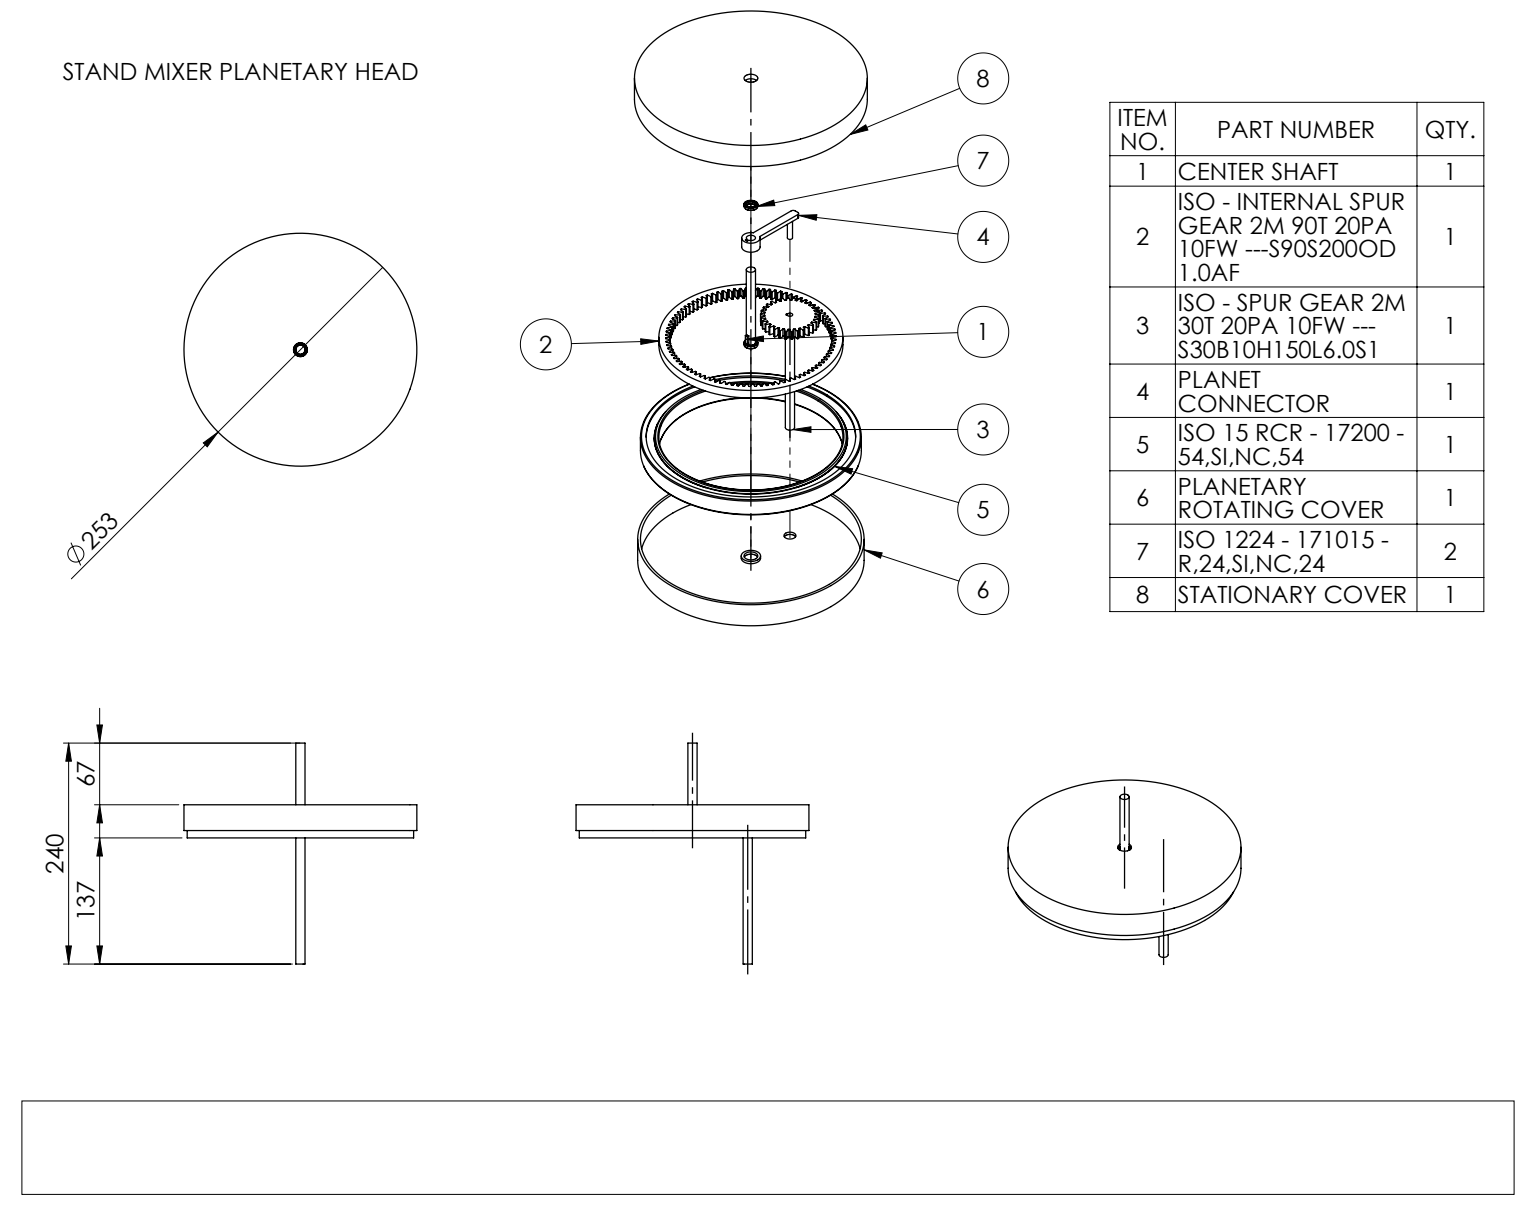
ISO-10303-21;
HEADER;
FILE_DESCRIPTION (('STEP AP214'),
    '1' );
FILE_NAME ('BR-820',
    '2026-09-30T13:58:28',
    ( '' ),
    ( '' ),
    'SwSTEP 2.0',
    'SolidWorks 2026',
    '' );
FILE_SCHEMA (( 'AUTOMOTIVE_DESIGN' ));
ENDSEC;

DATA;
#1 = VERTEX_POINT ( 'NONE', #11430 ) ;
#2 = DIRECTION ( 'NONE',  ( 1.000000000000000000, 0.000000000000000000, 0.000000000000000000 ) ) ;
#3 = ORIENTED_EDGE ( 'NONE', *, *, #13016, .T. ) ;
#4 = CARTESIAN_POINT ( 'NONE',  ( 10.00000000000000000, -41.21966518005896774, -82.80926399530329718 ) ) ;
#5 = EDGE_CURVE ( 'NONE', #21395, #6732, #6706, .T. ) ;
#6 = EDGE_CURVE ( 'NONE', #10604, #16693, #2923, .T. ) ;
#7 = EDGE_CURVE ( 'NONE', #1807, #19086, #14294, .T. ) ;
#8 = PLANE ( 'NONE',  #10324 ) ;
#9 = EDGE_CURVE ( 'NONE', #17849, #4256, #16629, .T. ) ;
#10 = DIRECTION ( 'NONE',  ( 0.000000000000000000, -0.8660254037844328234, -0.5000000000000101030 ) ) ;
#11 = DIRECTION ( 'NONE',  ( -1.000000000000000000, 0.000000000000000000, 0.000000000000000000 ) ) ;
#12 = AXIS2_PLACEMENT_3D ( 'NONE', #9946, #1451, #14823 ) ;
#13 = FACE_OUTER_BOUND ( 'NONE', #21140, .T. ) ;
#14 = CARTESIAN_POINT ( 'NONE',  ( 10.00000000000000000, 10.41137886060228901, -91.91321010181836471 ) ) ;
#15 = ORIENTED_EDGE ( 'NONE', *, *, #3774, .T. ) ;
#16 = LINE ( 'NONE', #18466, #6212 ) ;
#17 = EDGE_CURVE ( 'NONE', #14755, #17637, #4430, .T. ) ;
#18 = ORIENTED_EDGE ( 'NONE', *, *, #6903, .T. ) ;
#19 = ORIENTED_EDGE ( 'NONE', *, *, #690, .T. ) ;
#20 = ADVANCED_FACE ( 'NONE', ( #18069 ), #19725, .F. ) ;
#21 = CYLINDRICAL_SURFACE ( 'NONE', #38, 45.00000000000000000 ) ;
#22 = ORIENTED_EDGE ( 'NONE', *, *, #21258, .T. ) ;
#23 = CIRCLE ( 'NONE', #12352, 32.00000000000000000 ) ;
#24 = CYLINDRICAL_SURFACE ( 'NONE', #8070, 11.99999999999999822 ) ;
#25 = ORIENTED_EDGE ( 'NONE', *, *, #3908, .T. ) ;
#26 = ORIENTED_EDGE ( 'NONE', *, *, #547, .T. ) ;
#27 = DIRECTION ( 'NONE',  ( 0.000000000000000000, -0.2079116908177664202, 0.9781476007338040235 ) ) ;
#28 = ORIENTED_EDGE ( 'NONE', *, *, #6517, .T. ) ;
#29 = EDGE_CURVE ( 'NONE', #3387, #1233, #12896, .T. ) ;
#30 = DIRECTION ( 'NONE',  ( 1.000000000000000000, 0.000000000000000000, 0.000000000000000000 ) ) ;
#31 = EDGE_CURVE ( 'NONE', #17610, #10261, #11843, .T. ) ;
#32 = DIRECTION ( 'NONE',  ( 0.000000000000000000, 0.000000000000000000, -1.000000000000000000 ) ) ;
#33 = LINE ( 'NONE', #6780, #6309 ) ;
#34 = CARTESIAN_POINT ( 'NONE',  ( 0.000000000000000000, -19.83954325428713972, 82.71385593638686373 ) ) ;
#35 = DIRECTION ( 'NONE',  ( 0.000000000000000000, 0.000000000000000000, 1.000000000000000000 ) ) ;
#36 = CARTESIAN_POINT ( 'NONE',  ( 10.00000000000000000, 29.47587714451147534, -82.91666097089093057 ) ) ;
#37 = FACE_OUTER_BOUND ( 'NONE', #13774, .T. ) ;
#38 = AXIS2_PLACEMENT_3D ( 'NONE', #6766, #13480, #9727 ) ;
#39 = ORIENTED_EDGE ( 'NONE', *, *, #420, .F. ) ;
#40 = ADVANCED_FACE ( 'NONE', ( #13087 ), #18195, .T. ) ;
#41 = EDGE_CURVE ( 'NONE', #15664, #20418, #3042, .T. ) ;
#42 = DIRECTION ( 'NONE',  ( 0.000000000000000000, 0.000000000000000000, 1.000000000000000000 ) ) ;
#43 = DIRECTION ( 'NONE',  ( -1.000000000000000000, 0.000000000000000000, 0.000000000000000000 ) ) ;
#44 = EDGE_LOOP ( 'NONE', ( #15562, #858, #14802, #18530 ) ) ;
#45 = EDGE_CURVE ( 'NONE', #3976, #18093, #12185, .T. ) ;
#46 = DIRECTION ( 'NONE',  ( -1.000000000000000000, -0.000000000000000000, -0.000000000000000000 ) ) ;
#47 = EDGE_LOOP ( 'NONE', ( #15509, #8289, #2794, #20756 ) ) ;
#48 = EDGE_CURVE ( 'NONE', #21500, #20174, #21008, .T. ) ;
#49 = VERTEX_POINT ( 'NONE', #8229 ) ;
#50 = CARTESIAN_POINT ( 'NONE',  ( 10.00000000000000000, -19.07277123396528395, -19.80970465344768172 ) ) ;
#51 = ORIENTED_EDGE ( 'NONE', *, *, #17728, .T. ) ;
#52 = VERTEX_POINT ( 'NONE', #11320 ) ;
#53 = DIRECTION ( 'NONE',  ( -1.000000000000000000, 0.000000000000000000, -0.000000000000000000 ) ) ;
#54 = FACE_OUTER_BOUND ( 'NONE', #7670, .T. ) ;
#55 = ORIENTED_EDGE ( 'NONE', *, *, #20082, .T. ) ;
#56 = EDGE_CURVE ( 'NONE', #13601, #12425, #16433, .T. ) ;
#57 = DIRECTION ( 'NONE',  ( -1.000000000000000000, 0.000000000000000000, -0.000000000000000000 ) ) ;
#58 = DIRECTION ( 'NONE',  ( 1.000000000000000000, -0.000000000000000000, 0.000000000000000000 ) ) ;
#59 = DIRECTION ( 'NONE',  ( 1.000000000000000000, 0.000000000000000000, 0.000000000000000000 ) ) ;
#60 = DIRECTION ( 'NONE',  ( -1.000000000000000000, -0.000000000000000000, -0.000000000000000000 ) ) ;
#61 = DIRECTION ( 'NONE',  ( 0.000000000000000000, -0.5877852522924797984, 0.8090169943749425663 ) ) ;
#62 = DIRECTION ( 'NONE',  ( 1.000000000000000000, 0.000000000000000000, -0.000000000000000000 ) ) ;
#63 = ORIENTED_EDGE ( 'NONE', *, *, #8306, .T. ) ;
#64 = DIRECTION ( 'NONE',  ( 1.000000000000000000, 0.000000000000000000, 0.000000000000000000 ) ) ;
#65 = CARTESIAN_POINT ( 'NONE',  ( 10.00000000000000000, 33.95793648385814123, 86.04239391578002483 ) ) ;
#66 = CIRCLE ( 'NONE', #8534, 44.99999999999999289 ) ;
#67 = ORIENTED_EDGE ( 'NONE', *, *, #11916, .T. ) ;
#68 = DIRECTION ( 'NONE',  ( -1.000000000000000000, 0.000000000000000000, 0.000000000000000000 ) ) ;
#69 = ORIENTED_EDGE ( 'NONE', *, *, #9047, .F. ) ;
#70 = DIRECTION ( 'NONE',  ( 0.000000000000000000, 0.000000000000000000, 1.000000000000000000 ) ) ;
#71 = ORIENTED_EDGE ( 'NONE', *, *, #21788, .F. ) ;
#72 = EDGE_CURVE ( 'NONE', #17227, #7603, #6261, .T. ) ;
#73 = DIRECTION ( 'NONE',  ( 1.000000000000000000, 0.000000000000000000, 0.000000000000000000 ) ) ;
#74 = AXIS2_PLACEMENT_3D ( 'NONE', #17668, #2628, #2518 ) ;
#75 = VERTEX_POINT ( 'NONE', #9649 ) ;
#76 = ORIENTED_EDGE ( 'NONE', *, *, #8491, .T. ) ;
#77 = ORIENTED_EDGE ( 'NONE', *, *, #16610, .F. ) ;
#78 = DIRECTION ( 'NONE',  ( 1.000000000000000000, 0.000000000000000000, 0.000000000000000000 ) ) ;
#79 = ORIENTED_EDGE ( 'NONE', *, *, #6135, .T. ) ;
#80 = DIRECTION ( 'NONE',  ( 0.000000000000000000, 0.000000000000000000, 1.000000000000000000 ) ) ;
#81 = CARTESIAN_POINT ( 'NONE',  ( -1.500000000000000000, -7.000000000000000000, 15.00000000000000000 ) ) ;
#82 = DIRECTION ( 'NONE',  ( -1.000000000000000000, -0.000000000000000000, -0.000000000000000000 ) ) ;
#83 = CARTESIAN_POINT ( 'NONE',  ( 0.000000000000000000, -71.72924546249915068, -45.71766382684744201 ) ) ;
#84 = CARTESIAN_POINT ( 'NONE',  ( 10.00000000000000000, 0.000000000000000000, 0.000000000000000000 ) ) ;
#85 = AXIS2_PLACEMENT_3D ( 'NONE', #19345, #19670, #5876 ) ;
#86 = DIRECTION ( 'NONE',  ( 1.000000000000000000, 0.000000000000000000, 0.000000000000000000 ) ) ;
#87 = CARTESIAN_POINT ( 'NONE',  ( 10.00000000000000000, 0.000000000000000000, 0.000000000000000000 ) ) ;
#88 = CARTESIAN_POINT ( 'NONE',  ( 1.500000000000000000, -4.769696007084728073, 5.000000000000004441 ) ) ;
#89 = AXIS2_PLACEMENT_3D ( 'NONE', #19050, #14810, #11160 ) ;
#90 = DIRECTION ( 'NONE',  ( 1.000000000000000000, 0.000000000000000000, 0.000000000000000000 ) ) ;
#91 = CIRCLE ( 'NONE', #1856, 113.8250000000000171 ) ;
#92 = CARTESIAN_POINT ( 'NONE',  ( 0.000000000000000000, 100.0000000000000000, 0.000000000000000000 ) ) ;
#93 = ORIENTED_EDGE ( 'NONE', *, *, #13098, .F. ) ;
#94 = DIRECTION ( 'NONE',  ( -1.000000000000000000, -0.000000000000000000, -0.000000000000000000 ) ) ;
#95 = ADVANCED_FACE ( 'NONE', ( #16404 ), #1281, .F. ) ;
#96 = ORIENTED_EDGE ( 'NONE', *, *, #16353, .T. ) ;
#97 = FACE_OUTER_BOUND ( 'NONE', #19289, .T. ) ;
#98 = ORIENTED_EDGE ( 'NONE', *, *, #11209, .F. ) ;
#99 = CIRCLE ( 'NONE', #20908, 27.49900000000000233 ) ;
#100 = ORIENTED_EDGE ( 'NONE', *, *, #14180, .F. ) ;
#101 = PRODUCT_DEFINITION ( 'UNKNOWN', '', #429, #16859 ) ;
#102 = ORIENTED_EDGE ( 'NONE', *, *, #14178, .T. ) ;
#103 = CYLINDRICAL_SURFACE ( 'NONE', #17608, 88.00000000000000000 ) ;
#104 = CIRCLE ( 'NONE', #9604, 12.00000000000000000 ) ;
#105 = EDGE_LOOP ( 'NONE', ( #14807, #14622, #2671, #8655 ) ) ;
#106 = DIRECTION ( 'NONE',  ( 0.000000000000000000, 0.000000000000000000, 1.000000000000000000 ) ) ;
#107 = CARTESIAN_POINT ( 'NONE',  ( 5.000000000000000000, -30.71797041605752554, -82.46457599186584275 ) ) ;
#108 = AXIS2_PLACEMENT_3D ( 'NONE', #5672, #376, #480 ) ;
#109 = DIRECTION ( 'NONE',  ( -0.000000000000000000, -0.000000000000000000, 1.000000000000000000 ) ) ;
#110 = DIRECTION ( 'NONE',  ( -1.000000000000000000, 0.000000000000000000, 0.000000000000000000 ) ) ;
#111 = CYLINDRICAL_SURFACE ( 'NONE', #16029, 92.50100000000000477 ) ;
#112 = FACE_OUTER_BOUND ( 'NONE', #11461, .T. ) ;
#113 = DIRECTION ( 'NONE',  ( 0.000000000000000000, 0.000000000000000000, 1.000000000000000000 ) ) ;
#114 = CIRCLE ( 'NONE', #16698, 45.00000000000000711 ) ;
#115 = ORIENTED_EDGE ( 'NONE', *, *, #14200, .T. ) ;
#116 = DIRECTION ( 'NONE',  ( -1.000000000000000000, 0.000000000000000000, 0.000000000000000000 ) ) ;
#117 = CIRCLE ( 'NONE', #19528, 32.00000000000000000 ) ;
#118 = EDGE_CURVE ( 'NONE', #7770, #17965, #10413, .T. ) ;
#119 = EDGE_LOOP ( 'NONE', ( #6288, #20757, #6100, #17161 ) ) ;
#120 = CIRCLE ( 'NONE', #16359, 44.99999999999999289 ) ;
#121 = ORIENTED_EDGE ( 'NONE', *, *, #11165, .T. ) ;
#122 = CARTESIAN_POINT ( 'NONE',  ( 10.00000000000000000, 66.01871308925549897, -64.79170103522952218 ) ) ;
#123 = AXIS2_PLACEMENT_3D ( 'NONE', #20145, #6454, #4998 ) ;
#124 = ORIENTED_EDGE ( 'NONE', *, *, #16480, .F. ) ;
#125 = FACE_OUTER_BOUND ( 'NONE', #9793, .T. ) ;
#126 = ORIENTED_EDGE ( 'NONE', *, *, #4189, .T. ) ;
#127 = ORIENTED_EDGE ( 'NONE', *, *, #547, .F. ) ;
#128 = EDGE_CURVE ( 'NONE', #16693, #4447, #1608, .T. ) ;
#129 = FACE_OUTER_BOUND ( 'NONE', #11446, .T. ) ;
#130 = VECTOR ( 'NONE', #16734, 1000.000000000000000 ) ;
#131 = ORIENTED_EDGE ( 'NONE', *, *, #18244, .T. ) ;
#132 = DIRECTION ( 'NONE',  ( 0.000000000000000000, 0.000000000000000000, 1.000000000000000000 ) ) ;
#133 = EDGE_CURVE ( 'NONE', #20413, #2378, #1921, .T. ) ;
#134 = CIRCLE ( 'NONE', #12473, 5.100000000000000533 ) ;
#135 = CARTESIAN_POINT ( 'NONE',  ( -1.500000000000000000, -7.000000000000000000, 15.00000000000000000 ) ) ;
#136 = DIRECTION ( 'NONE',  ( 1.000000000000000000, 0.000000000000000000, 0.000000000000000000 ) ) ;
#137 = CARTESIAN_POINT ( 'NONE',  ( 0.000000000000000000, -36.60317927562525853, -76.78148674856802813 ) ) ;
#138 = CIRCLE ( 'NONE', #20266, 92.50100000000000477 ) ;
#139 = PLANE ( 'NONE',  #5077 ) ;
#140 = CARTESIAN_POINT ( 'NONE',  ( -90.00000000000000000, 0.000000000000000000, 0.000000000000000000 ) ) ;
#141 = DIRECTION ( 'NONE',  ( 0.000000000000000000, 0.2079116908177531808, 0.9781476007338069101 ) ) ;
#142 = VERTEX_POINT ( 'NONE', #1713 ) ;
#143 = EDGE_CURVE ( 'NONE', #8340, #1182, #890, .T. ) ;
#144 = EDGE_CURVE ( 'NONE', #2079, #18856, #6208, .T. ) ;
#145 = EDGE_CURVE ( 'NONE', #8013, #10982, #9353, .T. ) ;
#146 = DIRECTION ( 'NONE',  ( 1.000000000000000000, -0.000000000000000000, -0.000000000000000000 ) ) ;
#147 = VECTOR ( 'NONE', #20842, 1000.000000000000000 ) ;
#148 = ADVANCED_FACE ( 'NONE', ( #13522 ), #13849, .F. ) ;
#149 = CARTESIAN_POINT ( 'NONE',  ( 126.5000000000000000, 0.000000000000000000, -3.000000000000000000 ) ) ;
#150 = ORIENTED_EDGE ( 'NONE', *, *, #2176, .F. ) ;
#151 = CARTESIAN_POINT ( 'NONE',  ( 0.000000000000000000, -2.208823992044743445, 85.03123271466935762 ) ) ;
#152 = ORIENTED_EDGE ( 'NONE', *, *, #8425, .F. ) ;
#153 = CIRCLE ( 'NONE', #7560, 120.0000000000000568 ) ;
#154 = FILL_AREA_STYLE ('',( #18612 ) ) ;
#155 = VERTEX_POINT ( 'NONE', #6910 ) ;
#156 = LINE ( 'NONE', #19142, #3295 ) ;
#157 = ORIENTED_EDGE ( 'NONE', *, *, #5783, .T. ) ;
#158 = ORIENTED_EDGE ( 'NONE', *, *, #20800, .T. ) ;
#159 = CARTESIAN_POINT ( 'NONE',  ( -1.500000000000001332, 0.000000000000000000, 0.000000000000000000 ) ) ;
#160 = FACE_OUTER_BOUND ( 'NONE', #8742, .T. ) ;
#161 = ORIENTED_EDGE ( 'NONE', *, *, #12699, .T. ) ;
#162 = EDGE_CURVE ( 'NONE', #8199, #7224, #9947, .T. ) ;
#163 = VECTOR ( 'NONE', #1366, 1000.000000000000000 ) ;
#164 = CARTESIAN_POINT ( 'NONE',  ( 10.00000000000000000, 45.60224695560681596, -80.47900393021679122 ) ) ;
#165 = FACE_OUTER_BOUND ( 'NONE', #7515, .T. ) ;
#166 = AXIS2_PLACEMENT_3D ( 'NONE', #4020, #2367, #12315 ) ;
#167 = DIRECTION ( 'NONE',  ( -1.000000000000000000, -0.000000000000000000, -0.000000000000000000 ) ) ;
#168 = CARTESIAN_POINT ( 'NONE',  ( 0.000000000000000000, 0.000000000000000000, 0.000000000000000000 ) ) ;
#169 = DIRECTION ( 'NONE',  ( 1.000000000000000000, 0.000000000000000000, 0.000000000000000000 ) ) ;
#170 = EDGE_CURVE ( 'NONE', #2883, #19416, #16664, .T. ) ;
#171 = CARTESIAN_POINT ( 'NONE',  ( 5.000000000000000000, -56.05743251323904985, 67.83483072893783117 ) ) ;
#172 = AXIS2_PLACEMENT_3D ( 'NONE', #13423, #20277, #18409 ) ;
#173 = VERTEX_POINT ( 'NONE', #20274 ) ;
#174 = VECTOR ( 'NONE', #10367, 1000.000000000000000 ) ;
#175 = ADVANCED_FACE ( 'NONE', ( #54 ), #18832, .T. ) ;
#176 = CARTESIAN_POINT ( 'NONE',  ( 10.00000000000000000, 27.87320266523557777, 88.20158487341770126 ) ) ;
#177 = DIRECTION ( 'NONE',  ( -1.000000000000000000, -0.000000000000000000, -0.000000000000000000 ) ) ;
#178 = ORIENTED_EDGE ( 'NONE', *, *, #6724, .F. ) ;
#179 = DIRECTION ( 'NONE',  ( -1.000000000000000000, -0.000000000000000000, -0.000000000000000000 ) ) ;
#180 = EDGE_LOOP ( 'NONE', ( #20881, #18064, #12670, #4609 ) ) ;
#181 = AXIS2_PLACEMENT_3D ( 'NONE', #12579, #19535, #9476 ) ;
#182 = EDGE_CURVE ( 'NONE', #12268, #14735, #15959, .T. ) ;
#183 = CARTESIAN_POINT ( 'NONE',  ( 10.00000000000000000, -56.34908017029516714, -63.71789861856507997 ) ) ;
#184 = AXIS2_PLACEMENT_3D ( 'NONE', #4735, #1644, #19987 ) ;
#185 = FACE_OUTER_BOUND ( 'NONE', #19072, .T. ) ;
#186 = ORIENTED_EDGE ( 'NONE', *, *, #21572, .F. ) ;
#187 = CARTESIAN_POINT ( 'NONE',  ( 10.00000000000000000, 0.000000000000000000, 0.000000000000000000 ) ) ;
#188 = AXIS2_PLACEMENT_3D ( 'NONE', #7103, #5656, #15592 ) ;
#189 = ORIENTED_EDGE ( 'NONE', *, *, #5432, .T. ) ;
#190 = EDGE_LOOP ( 'NONE', ( #15961, #11977 ) ) ;
#191 = ORIENTED_EDGE ( 'NONE', *, *, #16743, .F. ) ;
#192 = LINE ( 'NONE', #6941, #8592 ) ;
#193 = CIRCLE ( 'NONE', #20307, 92.50100000000000477 ) ;
#194 = ORIENTED_EDGE ( 'NONE', *, *, #10939, .T. ) ;
#195 = LINE ( 'NONE', #7048, #17980 ) ;
#196 = FACE_OUTER_BOUND ( 'NONE', #2000, .T. ) ;
#197 = CARTESIAN_POINT ( 'NONE',  ( 10.00000000000000000, 75.27139873020885830, 53.76477968147838027 ) ) ;
#198 = DIRECTION ( 'NONE',  ( -1.000000000000000000, -0.000000000000000000, -0.000000000000000000 ) ) ;
#199 = CLOSED_SHELL ( 'NONE', ( #12068, #15575, #17594, #6767, #11084, #7759, #19088, #8385, #95 ) ) ;
#200 = ADVANCED_FACE ( 'NONE', ( #160 ), #12195, .F. ) ;
#201 = DIRECTION ( 'NONE',  ( -1.000000000000000000, 0.000000000000000000, 0.000000000000000000 ) ) ;
#202 = DIRECTION ( 'NONE',  ( 1.000000000000000000, 0.000000000000000000, 0.000000000000000000 ) ) ;
#203 = AXIS2_PLACEMENT_3D ( 'NONE', #2476, #711, #21255 ) ;
#204 = CARTESIAN_POINT ( 'NONE',  ( 0.000000000000000000, -65.83713140174766920, 58.39068529131174756 ) ) ;
#205 = CIRCLE ( 'NONE', #21358, 44.99999999999999289 ) ;
#206 = CARTESIAN_POINT ( 'NONE',  ( 10.00000000000000000, 0.000000000000000000, 0.000000000000000000 ) ) ;
#207 = EDGE_CURVE ( 'NONE', #13474, #6639, #1819, .T. ) ;
#208 = VECTOR ( 'NONE', #9875, 1000.000000000000000 ) ;
#209 = EDGE_CURVE ( 'NONE', #16392, #6661, #15284, .T. ) ;
#210 = FACE_OUTER_BOUND ( 'NONE', #13128, .T. ) ;
#211 = AXIS2_PLACEMENT_3D ( 'NONE', #19238, #20571, #8854 ) ;
#212 = CARTESIAN_POINT ( 'NONE',  ( 10.00000000000000888, 0.000000000000000000, 0.000000000000000000 ) ) ;
#213 = DIRECTION ( 'NONE',  ( 1.000000000000000000, 0.000000000000000000, 0.000000000000000000 ) ) ;
#214 = ORIENTED_EDGE ( 'NONE', *, *, #11490, .F. ) ;
#215 = VERTEX_POINT ( 'NONE', #17177 ) ;
#216 = LINE ( 'NONE', #10686, #17595 ) ;
#217 = ORIENTED_EDGE ( 'NONE', *, *, #17217, .F. ) ;
#218 = CIRCLE ( 'NONE', #7573, 92.50100000000000477 ) ;
#219 = EDGE_LOOP ( 'NONE', ( #5452, #14194, #8580, #6579 ) ) ;
#220 = AXIS2_PLACEMENT_3D ( 'NONE', #15734, #21034, #10973 ) ;
#221 = ORIENTED_EDGE ( 'NONE', *, *, #20358, .T. ) ;
#222 = DIRECTION ( 'NONE',  ( 0.000000000000000000, 0.000000000000000000, 1.000000000000000000 ) ) ;
#223 = ORIENTED_EDGE ( 'NONE', *, *, #9452, .F. ) ;
#224 = CARTESIAN_POINT ( 'NONE',  ( 10.00000000000000000, -81.97107881582179800, -22.71412948308650925 ) ) ;
#225 = DIRECTION ( 'NONE',  ( 0.000000000000000000, 0.000000000000000000, -1.000000000000000000 ) ) ;
#226 = CARTESIAN_POINT ( 'NONE',  ( 10.00000000000000000, 0.000000000000000000, 0.000000000000000000 ) ) ;
#227 = CARTESIAN_POINT ( 'NONE',  ( 10.00000000000000000, -27.26034713664092379, 4.817140289263571518 ) ) ;
#228 = DIRECTION ( 'NONE',  ( -1.000000000000000000, 0.000000000000000000, 0.000000000000000000 ) ) ;
#229 = CARTESIAN_POINT ( 'NONE',  ( 10.00000000000000000, 25.48117629651189375, 10.33947075754270095 ) ) ;
#230 = DIRECTION ( 'NONE',  ( 0.000000000000000000, 0.5877852522924741363, -0.8090169943749466741 ) ) ;
#231 = CIRCLE ( 'NONE', #6580, 12.00000000000000000 ) ;
#232 = ORIENTED_EDGE ( 'NONE', *, *, #45, .T. ) ;
#233 = CIRCLE ( 'NONE', #1637, 32.00000000000000000 ) ;
#234 = VECTOR ( 'NONE', #13783, 1000.000000000000000 ) ;
#235 = DIRECTION ( 'NONE',  ( -1.000000000000000000, 0.000000000000000000, 0.000000000000000000 ) ) ;
#236 = ORIENTED_EDGE ( 'NONE', *, *, #14894, .T. ) ;
#237 = ORIENTED_EDGE ( 'NONE', *, *, #7586, .T. ) ;
#238 = DIRECTION ( 'NONE',  ( 1.000000000000000000, 0.000000000000000000, 0.000000000000000000 ) ) ;
#239 = VERTEX_POINT ( 'NONE', #15611 ) ;
#240 = ORIENTED_EDGE ( 'NONE', *, *, #6283, .F. ) ;
#241 = DIRECTION ( 'NONE',  ( 0.000000000000000000, 0.000000000000000000, 1.000000000000000000 ) ) ;
#242 = ORIENTED_EDGE ( 'NONE', *, *, #31, .T. ) ;
#243 = AXIS2_PLACEMENT_3D ( 'NONE', #14900, #16894, #21541 ) ;
#244 = CIRCLE ( 'NONE', #21755, 92.50099999999999056 ) ;
#245 = DIRECTION ( 'NONE',  ( 0.000000000000000000, 0.000000000000000000, 1.000000000000000000 ) ) ;
#246 = DIRECTION ( 'NONE',  ( 0.000000000000000000, -0.4694715627858974671, 0.8829475928589232137 ) ) ;
#247 = DIRECTION ( 'NONE',  ( 1.000000000000000000, 0.000000000000000000, 0.000000000000000000 ) ) ;
#248 = EDGE_CURVE ( 'NONE', #18258, #6557, #15949, .T. ) ;
#249 = CARTESIAN_POINT ( 'NONE',  ( 10.00000000000000000, -91.49386717542229519, 13.61276130276963414 ) ) ;
#250 = CARTESIAN_POINT ( 'NONE',  ( 1.500000000000001332, 0.000000000000000000, 0.000000000000000000 ) ) ;
#251 = LINE ( 'NONE', #3457, #3152 ) ;
#252 = CYLINDRICAL_SURFACE ( 'NONE', #7349, 44.99999999999999289 ) ;
#253 = ORIENTED_EDGE ( 'NONE', *, *, #21351, .F. ) ;
#254 = EDGE_CURVE ( 'NONE', #9160, #4990, #3798, .T. ) ;
#255 = CIRCLE ( 'NONE', #10121, 11.99999999999999822 ) ;
#256 = CIRCLE ( 'NONE', #9062, 88.00000000000000000 ) ;
#257 = CIRCLE ( 'NONE', #4139, 92.50100000000001899 ) ;
#258 = DIRECTION ( 'NONE',  ( -1.000000000000000000, -0.000000000000000000, -0.000000000000000000 ) ) ;
#259 = DIRECTION ( 'NONE',  ( -1.000000000000000000, -0.000000000000000000, -0.000000000000000000 ) ) ;
#260 = ORIENTED_EDGE ( 'NONE', *, *, #20533, .T. ) ;
#261 = DIRECTION ( 'NONE',  ( -1.000000000000000000, -0.000000000000000000, -0.000000000000000000 ) ) ;
#262 = EDGE_LOOP ( 'NONE', ( #26, #4295, #8253, #16006 ) ) ;
#263 = ORIENTED_EDGE ( 'NONE', *, *, #7411, .F. ) ;
#264 = DIRECTION ( 'NONE',  ( -1.000000000000000000, -0.000000000000000000, -0.000000000000000000 ) ) ;
#265 = EDGE_LOOP ( 'NONE', ( #20128, #1055, #4125, #2694 ) ) ;
#266 = ORIENTED_EDGE ( 'NONE', *, *, #14983, .F. ) ;
#267 = CYLINDRICAL_SURFACE ( 'NONE', #10379, 44.99999999999999289 ) ;
#268 = CARTESIAN_POINT ( 'NONE',  ( 120.0000000000000000, 0.000000000000000000, -3.000000000000000000 ) ) ;
#269 = CIRCLE ( 'NONE', #5211, 44.99999999999999289 ) ;
#270 = CARTESIAN_POINT ( 'NONE',  ( 10.00000000000000000, -84.90234713953988432, 5.175025661883520200 ) ) ;
#271 = DIRECTION ( 'NONE',  ( 1.000000000000000000, 0.000000000000000000, 0.000000000000000000 ) ) ;
#272 = EDGE_CURVE ( 'NONE', #5074, #2288, #8772, .T. ) ;
#273 = CIRCLE ( 'NONE', #3803, 5.000000000000000000 ) ;
#274 = ADVANCED_FACE ( 'NONE', ( #3687 ), #15513, .F. ) ;
#275 = CARTESIAN_POINT ( 'NONE',  ( 0.000000000000000000, 0.000000000000000000, 0.000000000000000000 ) ) ;
#276 = EDGE_CURVE ( 'NONE', #11431, #4861, #15600, .T. ) ;
#277 = CARTESIAN_POINT ( 'NONE',  ( 10.00000000000000000, 0.000000000000000000, 0.000000000000000000 ) ) ;
#278 = AXIS2_PLACEMENT_3D ( 'NONE', #20316, #8268, #21854 ) ;
#279 = CARTESIAN_POINT ( 'NONE',  ( 0.000000000000000000, -61.60362715319078575, 62.84101464466223774 ) ) ;
#280 = CARTESIAN_POINT ( 'NONE',  ( 5.000000000000002665, -83.89484365856928605, 26.56417150042919673 ) ) ;
#281 = ADVANCED_FACE ( 'NONE', ( #12804 ), #21549, .F. ) ;
#282 = VERTEX_POINT ( 'NONE', #6088 ) ;
#283 = AXIS2_PLACEMENT_3D ( 'NONE', #3990, #20791, #1007 ) ;
#284 = FACE_OUTER_BOUND ( 'NONE', #6940, .T. ) ;
#285 = LINE ( 'NONE', #7031, #6929 ) ;
#286 = VERTEX_POINT ( 'NONE', #2978 ) ;
#287 = CARTESIAN_POINT ( 'NONE',  ( 5.000000000000000000, 87.96697768756401103, -2.410567674970879981 ) ) ;
#288 = EDGE_CURVE ( 'NONE', #3210, #16203, #21321, .T. ) ;
#289 = VERTEX_POINT ( 'NONE', #1331 ) ;
#290 = VECTOR ( 'NONE', #16490, 1000.000000000000000 ) ;
#291 = VECTOR ( 'NONE', #5677, 1000.000000000000000 ) ;
#292 = CARTESIAN_POINT ( 'NONE',  ( 10.00000000000000000, 0.000000000000000000, 0.000000000000000000 ) ) ;
#293 = AXIS2_PLACEMENT_3D ( 'NONE', #2385, #14534, #16196 ) ;
#294 = DIRECTION ( 'NONE',  ( -1.000000000000000000, 0.000000000000000000, 0.000000000000000000 ) ) ;
#295 = CIRCLE ( 'NONE', #15093, 7.500000000000021316 ) ;
#296 = ORIENTED_EDGE ( 'NONE', *, *, #20800, .F. ) ;
#297 = DIRECTION ( 'NONE',  ( -1.000000000000000000, -0.000000000000000000, 0.000000000000000000 ) ) ;
#298 = EDGE_CURVE ( 'NONE', #2674, #6765, #4540, .T. ) ;
#299 = ORIENTED_EDGE ( 'NONE', *, *, #7580, .F. ) ;
#300 = EDGE_LOOP ( 'NONE', ( #21001, #13570, #8396, #414 ) ) ;
#301 = VERTEX_POINT ( 'NONE', #21219 ) ;
#302 = CARTESIAN_POINT ( 'NONE',  ( -10.00000000000000888, 0.000000000000000000, 0.000000000000000000 ) ) ;
#303 = ORIENTED_EDGE ( 'NONE', *, *, #3809, .F. ) ;
#304 = CARTESIAN_POINT ( 'NONE',  ( 0.000000000000000000, 0.000000000000000000, 0.000000000000000000 ) ) ;
#305 = FACE_OUTER_BOUND ( 'NONE', #10474, .T. ) ;
#306 = DIRECTION ( 'NONE',  ( 0.000000000000000000, 0.000000000000000000, 1.000000000000000000 ) ) ;
#307 = DIRECTION ( 'NONE',  ( 1.000000000000000000, 0.000000000000000000, 0.000000000000000000 ) ) ;
#308 = DIRECTION ( 'NONE',  ( -1.000000000000000000, -0.000000000000000000, 0.000000000000000000 ) ) ;
#309 = DIRECTION ( 'NONE',  ( 1.000000000000000000, 0.000000000000000000, 0.000000000000000000 ) ) ;
#310 = CIRCLE ( 'NONE', #12639, 44.99999999999999289 ) ;
#311 = ADVANCED_FACE ( 'NONE', ( #6322 ), #16244, .F. ) ;
#312 = AXIS2_PLACEMENT_3D ( 'NONE', #17991, #11339, #16213 ) ;
#313 = CARTESIAN_POINT ( 'NONE',  ( -1.400000000000000577, 0.000000000000000000, -7.400000000000019895 ) ) ;
#314 = CARTESIAN_POINT ( 'NONE',  ( 0.000000000000000000, -46.89573839703331259, 79.73220629831473616 ) ) ;
#315 = AXIS2_PLACEMENT_3D ( 'NONE', #21324, #3204, #1444 ) ;
#316 = ORIENTED_EDGE ( 'NONE', *, *, #15812, .F. ) ;
#317 = VECTOR ( 'NONE', #1446, 1000.000000000000000 ) ;
#318 = FACE_OUTER_BOUND ( 'NONE', #13916, .T. ) ;
#319 = DIRECTION ( 'NONE',  ( 1.000000000000000000, 0.000000000000000000, 0.000000000000000000 ) ) ;
#320 = DIRECTION ( 'NONE',  ( -1.000000000000000000, -0.000000000000000000, 0.000000000000000000 ) ) ;
#321 = EDGE_CURVE ( 'NONE', #616, #3222, #16347, .T. ) ;
#322 = ORIENTED_EDGE ( 'NONE', *, *, #9631, .T. ) ;
#323 = ORIENTED_EDGE ( 'NONE', *, *, #14086, .T. ) ;
#324 = AXIS2_PLACEMENT_3D ( 'NONE', #2500, #12657, #2719 ) ;
#325 = CARTESIAN_POINT ( 'NONE',  ( 10.00000000000000000, -78.83848282823942100, 48.38314403117473006 ) ) ;
#326 = ADVANCED_FACE ( 'NONE', ( #19444 ), #4645, .F. ) ;
#327 = ORIENTED_EDGE ( 'NONE', *, *, #5685, .T. ) ;
#328 = AXIS2_PLACEMENT_3D ( 'NONE', #9035, #9242, #14226 ) ;
#329 = ORIENTED_EDGE ( 'NONE', *, *, #14866, .F. ) ;
#330 = CIRCLE ( 'NONE', #4199, 123.0000000000000000 ) ;
#331 = EDGE_CURVE ( 'NONE', #10029, #19516, #19552, .T. ) ;
#332 = AXIS2_PLACEMENT_3D ( 'NONE', #13001, #21404, #16426 ) ;
#333 = AXIS2_PLACEMENT_3D ( 'NONE', #15679, #658, #762 ) ;
#334 = ADVANCED_FACE ( 'NONE', ( #9495 ), #1106, .F. ) ;
#335 = ORIENTED_EDGE ( 'NONE', *, *, #9621, .F. ) ;
#336 = DIRECTION ( 'NONE',  ( 1.000000000000000000, 0.000000000000000000, 0.000000000000000000 ) ) ;
#337 = ORIENTED_EDGE ( 'NONE', *, *, #5445, .T. ) ;
#338 = CARTESIAN_POINT ( 'NONE',  ( 0.000000000000000000, -13.56333590713994575, -28.98337314858449076 ) ) ;
#339 = DIRECTION ( 'NONE',  ( 0.000000000000000000, -0.6946583704590034714, 0.7193398003386451967 ) ) ;
#340 = DIRECTION ( 'NONE',  ( 0.000000000000000000, 1.224646799147354933E-16, 1.000000000000000000 ) ) ;
#341 = DIRECTION ( 'NONE',  ( 1.000000000000000000, 0.000000000000000000, 0.000000000000000000 ) ) ;
#342 = EDGE_CURVE ( 'NONE', #6864, #16595, #7844, .T. ) ;
#343 = CARTESIAN_POINT ( 'NONE',  ( -5.000000000000000000, 70.00000000000000000, 9.999999999999998224 ) ) ;
#344 = CARTESIAN_POINT ( 'NONE',  ( 0.000000000000000000, 12.46320060045762013, -29.47318494484016327 ) ) ;
#345 = DIRECTION ( 'NONE',  ( 0.000000000000000000, 0.000000000000000000, -1.000000000000000000 ) ) ;
#346 = DIRECTION ( 'NONE',  ( 1.000000000000000000, -0.000000000000000000, -0.000000000000000000 ) ) ;
#347 = CIRCLE ( 'NONE', #5282, 88.00000000000000000 ) ;
#348 = AXIS2_PLACEMENT_3D ( 'NONE', #8886, #10652, #17196 ) ;
#349 = ORIENTED_EDGE ( 'NONE', *, *, #11633, .F. ) ;
#350 = DIRECTION ( 'NONE',  ( 0.000000000000000000, 0.000000000000000000, 1.000000000000000000 ) ) ;
#351 = ORIENTED_EDGE ( 'NONE', *, *, #3701, .F. ) ;
#352 = ORIENTED_EDGE ( 'NONE', *, *, #15867, .T. ) ;
#353 = DIRECTION ( 'NONE',  ( -1.000000000000000000, 0.000000000000000000, -0.000000000000000000 ) ) ;
#354 = ORIENTED_EDGE ( 'NONE', *, *, #19846, .T. ) ;
#355 = ORIENTED_EDGE ( 'NONE', *, *, #9307, .T. ) ;
#356 = CARTESIAN_POINT ( 'NONE',  ( 10.00000000000000000, 0.000000000000000000, 0.000000000000000000 ) ) ;
#357 = ORIENTED_EDGE ( 'NONE', *, *, #9039, .T. ) ;
#358 = CIRCLE ( 'NONE', #2121, 27.49900000000000944 ) ;
#359 = CIRCLE ( 'NONE', #4230, 27.49900000000000233 ) ;
#360 = DIRECTION ( 'NONE',  ( 0.000000000000000000, 0.000000000000000000, 1.000000000000000000 ) ) ;
#361 = CARTESIAN_POINT ( 'NONE',  ( 10.00000000000000000, -27.26034713664092379, -7.182859710736426706 ) ) ;
#362 = CARTESIAN_POINT ( 'NONE',  ( 10.00000000000000000, -86.77540292929711541, 14.62974526292689426 ) ) ;
#363 = DIRECTION ( 'NONE',  ( 0.000000000000000000, 0.000000000000000000, 1.000000000000000000 ) ) ;
#364 = DIRECTION ( 'NONE',  ( 0.000000000000000000, 0.000000000000000000, 1.000000000000000000 ) ) ;
#365 = DIRECTION ( 'NONE',  ( -1.000000000000000000, 0.000000000000000000, 0.000000000000000000 ) ) ;
#366 = DIRECTION ( 'NONE',  ( 0.000000000000000000, 0.5877852522924742473, -0.8090169943749465631 ) ) ;
#367 = ORIENTED_EDGE ( 'NONE', *, *, #16193, .F. ) ;
#368 = CIRCLE ( 'NONE', #4963, 44.99999999999998579 ) ;
#369 = DIRECTION ( 'NONE',  ( 0.000000000000000000, -0.8660254037844432595, 0.4999999999999920064 ) ) ;
#370 = DIRECTION ( 'NONE',  ( 1.000000000000000000, 0.000000000000000000, 0.000000000000000000 ) ) ;
#371 = ORIENTED_EDGE ( 'NONE', *, *, #13234, .F. ) ;
#372 = EDGE_CURVE ( 'NONE', #3326, #21836, #19668, .T. ) ;
#373 = DIRECTION ( 'NONE',  ( -1.000000000000000000, -0.000000000000000000, -0.000000000000000000 ) ) ;
#374 = VERTEX_POINT ( 'NONE', #17387 ) ;
#375 =( NAMED_UNIT ( * ) PLANE_ANGLE_UNIT ( ) SI_UNIT ( $, .RADIAN. ) );
#376 = DIRECTION ( 'NONE',  ( -1.000000000000000000, 0.000000000000000000, 0.000000000000000000 ) ) ;
#377 = ORIENTED_EDGE ( 'NONE', *, *, #8030, .T. ) ;
#378 = VERTEX_POINT ( 'NONE', #9266 ) ;
#379 = CARTESIAN_POINT ( 'NONE',  ( 10.00000000000000000, -57.06999622551850138, 66.98518889142063415 ) ) ;
#380 = DIRECTION ( 'NONE',  ( 1.000000000000000000, 0.000000000000000000, 0.000000000000000000 ) ) ;
#381 = PRODUCT_DEFINITION ( 'UNKNOWN', '', #13101, #3862 ) ;
#382 = CARTESIAN_POINT ( 'NONE',  ( 0.000000000000000000, -75.45728100697627383, 39.26051685139039193 ) ) ;
#383 = DIRECTION ( 'NONE',  ( 0.000000000000000000, 0.000000000000000000, 1.000000000000000000 ) ) ;
#384 = FACE_OUTER_BOUND ( 'NONE', #4779, .T. ) ;
#385 = AXIS2_PLACEMENT_3D ( 'NONE', #3175, #1301, #4716 ) ;
#386 = CYLINDRICAL_SURFACE ( 'NONE', #20961, 44.99999999999999289 ) ;
#387 = DIRECTION ( 'NONE',  ( -1.000000000000000000, -0.000000000000000000, -0.000000000000000000 ) ) ;
#388 = LINE ( 'NONE', #20601, #18757 ) ;
#389 = VERTEX_POINT ( 'NONE', #4305 ) ;
#390 = CARTESIAN_POINT ( 'NONE',  ( 0.000000000000000000, -79.66702613806754130, -29.80527447819517661 ) ) ;
#391 = ORIENTED_EDGE ( 'NONE', *, *, #16340, .T. ) ;
#392 = CARTESIAN_POINT ( 'NONE',  ( 10.00000000000000000, 19.83954325428771881, -82.71385593638672162 ) ) ;
#393 = VERTEX_POINT ( 'NONE', #883 ) ;
#394 = CARTESIAN_POINT ( 'NONE',  ( 10.00000000000000000, 28.15804365424197186, -1.358152127006073684 ) ) ;
#395 = EDGE_CURVE ( 'NONE', #9256, #19686, #11275, .T. ) ;
#396 = MECHANICAL_DESIGN_GEOMETRIC_PRESENTATION_REPRESENTATION (  '', ( #1101 ), #5694 ) ;
#397 = DIRECTION ( 'NONE',  ( 0.000000000000000000, 0.000000000000000000, -1.000000000000000000 ) ) ;
#398 = ORIENTED_EDGE ( 'NONE', *, *, #6942, .T. ) ;
#399 = ORIENTED_EDGE ( 'NONE', *, *, #18525, .T. ) ;
#400 = ORIENTED_EDGE ( 'NONE', *, *, #3209, .F. ) ;
#401 = ORIENTED_EDGE ( 'NONE', *, *, #14036, .F. ) ;
#402 = DIRECTION ( 'NONE',  ( 0.000000000000000000, -0.8660254037844328234, -0.5000000000000101030 ) ) ;
#403 = ORIENTED_EDGE ( 'NONE', *, *, #3916, .T. ) ;
#404 = DIRECTION ( 'NONE',  ( -1.000000000000000000, -0.000000000000000000, 0.000000000000000000 ) ) ;
#405 = CYLINDRICAL_SURFACE ( 'NONE', #13914, 88.00000000000000000 ) ;
#406 = DIRECTION ( 'NONE',  ( -1.000000000000000000, -0.000000000000000000, 0.000000000000000000 ) ) ;
#407 = DIRECTION ( 'NONE',  ( 1.000000000000000000, 0.000000000000000000, 0.000000000000000000 ) ) ;
#408 = DIRECTION ( 'NONE',  ( 0.000000000000000000, 0.000000000000000000, 1.000000000000000000 ) ) ;
#409 = CARTESIAN_POINT ( 'NONE',  ( 0.000000000000000000, 0.000000000000000000, 0.000000000000000000 ) ) ;
#410 = EDGE_CURVE ( 'NONE', #2166, #21782, #436, .T. ) ;
#411 = CIRCLE ( 'NONE', #3579, 113.8250000000000171 ) ;
#412 = FACE_OUTER_BOUND ( 'NONE', #20325, .T. ) ;
#413 = AXIS2_PLACEMENT_3D ( 'NONE', #19468, #6343, #19803 ) ;
#414 = ORIENTED_EDGE ( 'NONE', *, *, #12479, .F. ) ;
#415 = EDGE_CURVE ( 'NONE', #508, #14361, #20203, .T. ) ;
#416 = DIRECTION ( 'NONE',  ( -1.000000000000000000, 0.000000000000000000, -0.000000000000000000 ) ) ;
#417 = DIRECTION ( 'NONE',  ( 0.000000000000000000, 0.000000000000000000, -1.000000000000000000 ) ) ;
#418 = LINE ( 'NONE', #20634, #10815 ) ;
#419 = VERTEX_POINT ( 'NONE', #1003 ) ;
#420 = EDGE_CURVE ( 'NONE', #17054, #16203, #9590, .T. ) ;
#421 = CARTESIAN_POINT ( 'NONE',  ( -10.00000000000000000, 0.000000000000000000, 0.000000000000000000 ) ) ;
#422 = EDGE_CURVE ( 'NONE', #6705, #19466, #20900, .T. ) ;
#423 = EDGE_CURVE ( 'NONE', #1592, #10683, #10658, .T. ) ;
#424 = ORIENTED_EDGE ( 'NONE', *, *, #5191, .T. ) ;
#425 = DIRECTION ( 'NONE',  ( 1.000000000000000000, 0.000000000000000000, 0.000000000000000000 ) ) ;
#426 = EDGE_LOOP ( 'NONE', ( #2512, #10819, #21191, #16481 ) ) ;
#427 = EDGE_CURVE ( 'NONE', #19313, #4861, #15245, .T. ) ;
#428 = VERTEX_POINT ( 'NONE', #21651 ) ;
#429 = PRODUCT_DEFINITION_FORMATION_WITH_SPECIFIED_SOURCE ( 'ANY', '', #11974, .NOT_KNOWN. ) ;
#430 = ORIENTED_EDGE ( 'NONE', *, *, #8428, .T. ) ;
#431 = CARTESIAN_POINT ( 'NONE',  ( 0.000000000000000000, -40.72878876293203376, 78.00747250042435610 ) ) ;
#432 = CARTESIAN_POINT ( 'NONE',  ( 5.000000000000000000, -30.24235385705231849, -10.45944707835137777 ) ) ;
#433 = CARTESIAN_POINT ( 'NONE',  ( 10.00000000000000000, 0.000000000000000000, 0.000000000000000000 ) ) ;
#434 = CARTESIAN_POINT ( 'NONE',  ( 8.899999999999989697, 1.238117913937974620E-14, 101.1000000000000512 ) ) ;
#435 = ADVANCED_FACE ( 'NONE', ( #5083 ), #5200, .F. ) ;
#436 = CIRCLE ( 'NONE', #3254, 92.50099999999999056 ) ;
#437 = CARTESIAN_POINT ( 'NONE',  ( 10.00000000000000000, 23.10190250628953379, -89.56973317806578905 ) ) ;
#438 = DIRECTION ( 'NONE',  ( 0.000000000000000000, -0.9993908270190959842, 0.03489949670249113678 ) ) ;
#439 = CARTESIAN_POINT ( 'NONE',  ( 0.000000000000000000, 83.48638250753266732, -27.82128566055030916 ) ) ;
#440 = EDGE_CURVE ( 'NONE', #16787, #1439, #11371, .T. ) ;
#441 = CARTESIAN_POINT ( 'NONE',  ( 10.00000000000000000, 51.76708072107885528, 67.49339815138510801 ) ) ;
#442 = ADVANCED_FACE ( 'NONE', ( #4975 ), #20117, .F. ) ;
#443 = CARTESIAN_POINT ( 'NONE',  ( 0.000000000000000000, -61.71252885873428085, 58.53847642588571887 ) ) ;
#444 = ORIENTED_EDGE ( 'NONE', *, *, #1345, .F. ) ;
#445 = EDGE_CURVE ( 'NONE', #19369, #15511, #13481, .T. ) ;
#446 = DIRECTION ( 'NONE',  ( -1.000000000000000000, 0.000000000000000000, -0.000000000000000000 ) ) ;
#447 = VERTEX_POINT ( 'NONE', #4 ) ;
#448 = VECTOR ( 'NONE', #10833, 1000.000000000000000 ) ;
#449 = EDGE_LOOP ( 'NONE', ( #5641, #4304, #5239, #6868 ) ) ;
#450 = ORIENTED_EDGE ( 'NONE', *, *, #11470, .F. ) ;
#451 = DIRECTION ( 'NONE',  ( 0.000000000000000000, 0.2079116908177599532, -0.9781476007338055778 ) ) ;
#452 = EDGE_CURVE ( 'NONE', #3829, #10685, #18573, .T. ) ;
#453 = VERTEX_POINT ( 'NONE', #15229 ) ;
#454 = VERTEX_POINT ( 'NONE', #1544 ) ;
#455 = AXIS2_PLACEMENT_3D ( 'NONE', #21743, #16562, #6840 ) ;
#456 = EDGE_CURVE ( 'NONE', #2112, #5619, #7500, .T. ) ;
#457 = CARTESIAN_POINT ( 'NONE',  ( 10.00000000000000000, 0.000000000000000000, 0.000000000000000000 ) ) ;
#458 = ORIENTED_EDGE ( 'NONE', *, *, #7475, .F. ) ;
#459 = DIRECTION ( 'NONE',  ( -1.000000000000000000, -0.000000000000000000, -0.000000000000000000 ) ) ;
#460 = CARTESIAN_POINT ( 'NONE',  ( 0.000000000000000000, 83.35585896458619004, 16.94078559807978124 ) ) ;
#461 = AXIS2_PLACEMENT_3D ( 'NONE', #4977, #18458, #3312 ) ;
#462 = DIRECTION ( 'NONE',  ( 0.000000000000000000, 0.000000000000000000, 1.000000000000000000 ) ) ;
#463 = DIRECTION ( 'NONE',  ( 0.000000000000000000, 0.000000000000000000, 1.000000000000000000 ) ) ;
#464 = CARTESIAN_POINT ( 'NONE',  ( 10.00000000000000000, 81.83745710415276164, 32.35167097270178260 ) ) ;
#465 = ADVANCED_FACE ( 'NONE', ( #3425 ), #3311, .T. ) ;
#466 = DIRECTION ( 'NONE',  ( 1.000000000000000000, 0.000000000000000000, 0.000000000000000000 ) ) ;
#467 = DIRECTION ( 'NONE',  ( 1.000000000000000000, 0.000000000000000000, 0.000000000000000000 ) ) ;
#468 = CARTESIAN_POINT ( 'NONE',  ( 0.000000000000000000, 0.000000000000000000, 0.000000000000000000 ) ) ;
#469 = CIRCLE ( 'NONE', #10677, 10.49999999999999822 ) ;
#470 = CIRCLE ( 'NONE', #16293, 5.612499999999999822 ) ;
#471 = ORIENTED_EDGE ( 'NONE', *, *, #2986, .T. ) ;
#472 = CIRCLE ( 'NONE', #10698, 88.00000000000000000 ) ;
#473 = EDGE_CURVE ( 'NONE', #20811, #14806, #13136, .T. ) ;
#474 = DIRECTION ( 'NONE',  ( 1.000000000000000000, -0.000000000000000000, -0.000000000000000000 ) ) ;
#475 = CARTESIAN_POINT ( 'NONE',  ( 10.00000000000000000, 0.000000000000000000, 0.000000000000000000 ) ) ;
#476 = ORIENTED_EDGE ( 'NONE', *, *, #19100, .F. ) ;
#477 = LINE ( 'NONE', #18723, #16771 ) ;
#478 = ORIENTED_EDGE ( 'NONE', *, *, #17582, .T. ) ;
#479 = VECTOR ( 'NONE', #8463, 1000.000000000000000 ) ;
#480 = DIRECTION ( 'NONE',  ( 0.000000000000000000, 0.000000000000000000, 1.000000000000000000 ) ) ;
#481 = VERTEX_POINT ( 'NONE', #13580 ) ;
#482 = ORIENTED_EDGE ( 'NONE', *, *, #12164, .F. ) ;
#483 = CARTESIAN_POINT ( 'NONE',  ( 0.000000000000000000, 0.000000000000000000, 0.000000000000000000 ) ) ;
#484 = DIRECTION ( 'NONE',  ( -1.000000000000000000, -0.000000000000000000, 0.000000000000000000 ) ) ;
#485 = CIRCLE ( 'NONE', #20594, 104.9000000000000341 ) ;
#486 = AXIS2_PLACEMENT_3D ( 'NONE', #4785, #9859, #11408 ) ;
#487 = CARTESIAN_POINT ( 'NONE',  ( 0.000000000000000000, 0.000000000000000000, 3.000000000000000000 ) ) ;
#488 = LINE ( 'NONE', #12200, #995 ) ;
#489 = DIRECTION ( 'NONE',  ( -1.000000000000000000, 0.000000000000000000, 0.000000000000000000 ) ) ;
#490 = CARTESIAN_POINT ( 'NONE',  ( -90.00000000000000000, 0.000000000000000000, 0.000000000000000000 ) ) ;
#491 = ADVANCED_FACE ( 'NONE', ( #3094 ), #1440, .F. ) ;
#492 = CARTESIAN_POINT ( 'NONE',  ( 9.999999999999994671, 0.000000000000000000, 0.000000000000000000 ) ) ;
#493 = DIRECTION ( 'NONE',  ( 1.000000000000000000, 0.000000000000000000, -0.000000000000000000 ) ) ;
#494 = AXIS2_PLACEMENT_3D ( 'NONE', #84, #10670, #5605 ) ;
#495 = EDGE_LOOP ( 'NONE', ( #11685, #11364, #5919, #15728 ) ) ;
#496 = CARTESIAN_POINT ( 'NONE',  ( -90.00000000000000000, 0.000000000000000000, -115.1000000000000227 ) ) ;
#497 = AXIS2_PLACEMENT_3D ( 'NONE', #13069, #4792, #16173 ) ;
#498 = EDGE_LOOP ( 'NONE', ( #15179, #10420, #7326, #14605 ) ) ;
#499 = TOROIDAL_SURFACE ( 'NONE', #15302, 5.633200000000004870, 0.02570000000000143697 ) ;
#500 = DIRECTION ( 'NONE',  ( -1.000000000000000000, 0.000000000000000000, -0.000000000000000000 ) ) ;
#501 = ORIENTED_EDGE ( 'NONE', *, *, #10543, .F. ) ;
#502 = DIRECTION ( 'NONE',  ( 1.000000000000000000, 0.000000000000000000, 0.000000000000000000 ) ) ;
#503 = CARTESIAN_POINT ( 'NONE',  ( 6.123233995736766282E-16, -5.000000000000000000, 100.0000000000000000 ) ) ;
#504 = EDGE_LOOP ( 'NONE', ( #15894, #8627, #3713, #2897 ) ) ;
#505 = CIRCLE ( 'NONE', #2264, 44.99999999999998579 ) ;
#506 = ORIENTED_EDGE ( 'NONE', *, *, #19036, .F. ) ;
#507 = ORIENTED_EDGE ( 'NONE', *, *, #5060, .F. ) ;
#508 = VERTEX_POINT ( 'NONE', #9825 ) ;
#509 = CARTESIAN_POINT ( 'NONE',  ( 0.000000000000000000, 78.04699792498210797, -49.64978465107211036 ) ) ;
#510 = VERTEX_POINT ( 'NONE', #6754 ) ;
#511 = AXIS2_PLACEMENT_3D ( 'NONE', #10667, #17317, #5821 ) ;
#512 = CARTESIAN_POINT ( 'NONE',  ( -8.000000000000007105, 1.284654492305574008E-14, 104.9000000000000341 ) ) ;
#513 = DIRECTION ( 'NONE',  ( -1.000000000000000000, -0.000000000000000000, 0.000000000000000000 ) ) ;
#514 = DIRECTION ( 'NONE',  ( 0.000000000000000000, -0.9945218953682744001, 0.1045284632676437286 ) ) ;
#515 = CARTESIAN_POINT ( 'NONE',  ( 10.00000000000000000, -46.89573839703219704, -79.73220629831536144 ) ) ;
#516 = CARTESIAN_POINT ( 'NONE',  ( 0.000000000000000000, 0.000000000000000000, 0.000000000000000000 ) ) ;
#517 = EDGE_CURVE ( 'NONE', #19516, #10855, #18813, .T. ) ;
#518 = LINE ( 'NONE', #17324, #20205 ) ;
#519 = ORIENTED_EDGE ( 'NONE', *, *, #15032, .F. ) ;
#520 = CARTESIAN_POINT ( 'NONE',  ( 0.000000000000000000, -19.83954325428602061, -82.71385593638713374 ) ) ;
#521 = AXIS2_PLACEMENT_3D ( 'NONE', #551, #12365, #12467 ) ;
#522 = DIRECTION ( 'NONE',  ( 0.000000000000000000, -0.4067366430757887175, -0.9135454576426059736 ) ) ;
#523 = AXIS2_PLACEMENT_3D ( 'NONE', #5294, #8493, #10353 ) ;
#524 = EDGE_CURVE ( 'NONE', #12679, #374, #13850, .T. ) ;
#525 = CIRCLE ( 'NONE', #18926, 32.00000000000000000 ) ;
#526 = DIRECTION ( 'NONE',  ( 0.000000000000000000, -1.954455116267202870E-14, -1.000000000000000000 ) ) ;
#528 = AXIS2_PLACEMENT_3D ( 'NONE', #1902, #8639, #3779 ) ;
#527 = AXIS2_PLACEMENT_3D ( 'NONE', #18273, #14833, #16166 ) ;
#529 = ORIENTED_EDGE ( 'NONE', *, *, #2959, .T. ) ;
#530 = DIRECTION ( 'NONE',  ( 0.000000000000000000, 0.000000000000000000, -1.000000000000000000 ) ) ;
#531 = ORIENTED_EDGE ( 'NONE', *, *, #20947, .F. ) ;
#532 = DIRECTION ( 'NONE',  ( 0.000000000000000000, 0.000000000000000000, -1.000000000000000000 ) ) ;
#533 = ORIENTED_EDGE ( 'NONE', *, *, #17872, .T. ) ;
#534 = ADVANCED_FACE ( 'NONE', ( #10157 ), #3200, .F. ) ;
#535 = VERTEX_POINT ( 'NONE', #6644 ) ;
#536 = VERTEX_POINT ( 'NONE', #13466 ) ;
#537 = DIRECTION ( 'NONE',  ( 0.000000000000000000, 0.000000000000000000, 1.000000000000000000 ) ) ;
#538 = ORIENTED_EDGE ( 'NONE', *, *, #2848, .F. ) ;
#539 = DIRECTION ( 'NONE',  ( 0.000000000000000000, 0.000000000000000000, -1.000000000000000000 ) ) ;
#540 = CYLINDRICAL_SURFACE ( 'NONE', #2987, 92.50100000000000477 ) ;
#541 = CARTESIAN_POINT ( 'NONE',  ( 0.000000000000000000, 57.06999622551805373, 66.98518889142101784 ) ) ;
#542 = AXIS2_PLACEMENT_3D ( 'NONE', #21181, #2611, #6162 ) ;
#543 = AXIS2_PLACEMENT_3D ( 'NONE', #17281, #13952, #2235 ) ;
#544 = CARTESIAN_POINT ( 'NONE',  ( 0.000000000000000000, 60.00000000000000000, -15.00000000000000000 ) ) ;
#545 = AXIS2_PLACEMENT_3D ( 'NONE', #9654, #1395, #11435 ) ;
#546 = AXIS2_PLACEMENT_3D ( 'NONE', #10508, #2124, #572 ) ;
#547 = EDGE_CURVE ( 'NONE', #16474, #10634, #16910, .T. ) ;
#548 = CARTESIAN_POINT ( 'NONE',  ( 10.00000000000000000, 69.25892805976512534, 49.38005998797868301 ) ) ;
#549 = EDGE_CURVE ( 'NONE', #481, #1387, #12460, .T. ) ;
#550 = CARTESIAN_POINT ( 'NONE',  ( -5.000000000000000000, 67.00000000000000000, 15.00000000000000000 ) ) ;
#551 = CARTESIAN_POINT ( 'NONE',  ( 10.00000000000000000, 0.000000000000000000, 0.000000000000000000 ) ) ;
#552 = EDGE_CURVE ( 'NONE', #19754, #4889, #9037, .T. ) ;
#553 = DIRECTION ( 'NONE',  ( 1.000000000000000000, -0.000000000000000000, -0.000000000000000000 ) ) ;
#554 = DIRECTION ( 'NONE',  ( -1.000000000000000000, 0.000000000000000000, 0.000000000000000000 ) ) ;
#555 = EDGE_CURVE ( 'NONE', #7130, #7194, #6103, .T. ) ;
#556 = ORIENTED_EDGE ( 'NONE', *, *, #17340, .T. ) ;
#557 = FACE_OUTER_BOUND ( 'NONE', #3741, .T. ) ;
#558 = ORIENTED_EDGE ( 'NONE', *, *, #12580, .T. ) ;
#559 = ORIENTED_EDGE ( 'NONE', *, *, #2768, .F. ) ;
#560 = CIRCLE ( 'NONE', #1979, 32.00000000000000000 ) ;
#561 = ORIENTED_EDGE ( 'NONE', *, *, #20234, .T. ) ;
#562 = EDGE_CURVE ( 'NONE', #6281, #4746, #2302, .T. ) ;
#563 = AXIS2_PLACEMENT_3D ( 'NONE', #8857, #15596, #14375 ) ;
#564 = CARTESIAN_POINT ( 'NONE',  ( -10.00000000000000000, 0.000000000000000000, 0.000000000000000000 ) ) ;
#565 = ORIENTED_EDGE ( 'NONE', *, *, #7928, .T. ) ;
#566 = ORIENTED_EDGE ( 'NONE', *, *, #12735, .T. ) ;
#567 = EDGE_CURVE ( 'NONE', #14361, #6281, #9246, .T. ) ;
#568 = CARTESIAN_POINT ( 'NONE',  ( 10.00000000000000000, 86.77540292929701593, 14.62974526292747868 ) ) ;
#569 = VERTEX_POINT ( 'NONE', #15459 ) ;
#570 = CYLINDRICAL_SURFACE ( 'NONE', #13210, 92.50100000000000477 ) ;
#571 = DIRECTION ( 'NONE',  ( 0.000000000000000000, 0.000000000000000000, 1.000000000000000000 ) ) ;
#572 = DIRECTION ( 'NONE',  ( 0.000000000000000000, 0.000000000000000000, 1.000000000000000000 ) ) ;
#573 = CARTESIAN_POINT ( 'NONE',  ( -10.00000000000000000, 0.000000000000000000, 0.000000000000000000 ) ) ;
#574 = AXIS2_PLACEMENT_3D ( 'NONE', #19114, #15472, #1997 ) ;
#575 = DIRECTION ( 'NONE',  ( 0.000000000000000000, 0.000000000000000000, 1.000000000000000000 ) ) ;
#576 = AXIS2_PLACEMENT_3D ( 'NONE', #16604, #1464, #10075 ) ;
#577 = DIRECTION ( 'NONE',  ( 0.000000000000000000, 0.000000000000000000, 1.000000000000000000 ) ) ;
#578 = DIRECTION ( 'NONE',  ( 1.000000000000000000, 0.000000000000000000, 0.000000000000000000 ) ) ;
#580 = CIRCLE ( 'NONE', #5471, 44.99999999999999289 ) ;
#579 = CARTESIAN_POINT ( 'NONE',  ( 10.00000000000000000, 0.000000000000000000, 0.000000000000000000 ) ) ;
#581 = EDGE_CURVE ( 'NONE', #14715, #6477, #17390, .T. ) ;
#582 = ORIENTED_EDGE ( 'NONE', *, *, #10536, .F. ) ;
#583 = DIRECTION ( 'NONE',  ( 0.000000000000000000, 0.5299192642331999048, 0.8480480961564291764 ) ) ;
#584 = EDGE_CURVE ( 'NONE', #11040, #9927, #13903, .T. ) ;
#585 = DIRECTION ( 'NONE',  ( 0.000000000000000000, -0.5877852522924632561, -0.8090169943749546677 ) ) ;
#586 = ORIENTED_EDGE ( 'NONE', *, *, #3118, .T. ) ;
#587 = FACE_OUTER_BOUND ( 'NONE', #12213, .T. ) ;
#588 = EDGE_CURVE ( 'NONE', #8553, #4990, #15267, .T. ) ;
#589 = VERTEX_POINT ( 'NONE', #541 ) ;
#590 = VECTOR ( 'NONE', #17368, 1000.000000000000000 ) ;
#591 = CARTESIAN_POINT ( 'NONE',  ( 0.000000000000000000, 0.000000000000000000, 0.000000000000000000 ) ) ;
#592 = FACE_OUTER_BOUND ( 'NONE', #14290, .T. ) ;
#593 = ORIENTED_EDGE ( 'NONE', *, *, #19598, .F. ) ;
#594 = ORIENTED_EDGE ( 'NONE', *, *, #1930, .F. ) ;
#595 = EDGE_CURVE ( 'NONE', #18348, #18539, #20217, .T. ) ;
#596 = DIRECTION ( 'NONE',  ( -1.000000000000000000, 0.000000000000000000, -0.000000000000000000 ) ) ;
#597 = EDGE_CURVE ( 'NONE', #6613, #715, #14016, .T. ) ;
#598 = DIRECTION ( 'NONE',  ( 0.000000000000000000, -0.5877852522924632561, -0.8090169943749545567 ) ) ;
#599 = DIRECTION ( 'NONE',  ( 1.000000000000000000, 0.000000000000000000, 0.000000000000000000 ) ) ;
#600 = DIRECTION ( 'NONE',  ( 1.000000000000000000, 0.000000000000000000, 0.000000000000000000 ) ) ;
#601 = DIRECTION ( 'NONE',  ( 1.000000000000000000, 0.000000000000000000, 0.000000000000000000 ) ) ;
#602 = DIRECTION ( 'NONE',  ( -1.000000000000000000, 0.000000000000000000, 0.000000000000000000 ) ) ;
#603 = CARTESIAN_POINT ( 'NONE',  ( 0.000000000000000000, 0.000000000000000000, 0.000000000000000000 ) ) ;
#604 = VECTOR ( 'NONE', #20554, 1000.000000000000000 ) ;
#605 = VECTOR ( 'NONE', #3170, 1000.000000000000000 ) ;
#606 = ORIENTED_EDGE ( 'NONE', *, *, #10944, .F. ) ;
#607 = DIRECTION ( 'NONE',  ( 0.000000000000000000, 0.000000000000000000, 1.000000000000000000 ) ) ;
#608 = ORIENTED_EDGE ( 'NONE', *, *, #11246, .T. ) ;
#609 = CARTESIAN_POINT ( 'NONE',  ( 10.00000000000000000, 14.02138820415029663, -83.89630571862271324 ) ) ;
#610 = VERTEX_POINT ( 'NONE', #10481 ) ;
#611 = DIRECTION ( 'NONE',  ( 0.000000000000000000, 0.000000000000000000, 1.000000000000000000 ) ) ;
#612 = FACE_OUTER_BOUND ( 'NONE', #18647, .T. ) ;
#613 = ORIENTED_EDGE ( 'NONE', *, *, #13922, .F. ) ;
#614 = CIRCLE ( 'NONE', #16845, 44.99999999999999289 ) ;
#615 = EDGE_LOOP ( 'NONE', ( #5922, #19113 ) ) ;
#616 = VERTEX_POINT ( 'NONE', #12037 ) ;
#617 = AXIS2_PLACEMENT_3D ( 'NONE', #12857, #4142, #19606 ) ;
#618 = ORIENTED_EDGE ( 'NONE', *, *, #20802, .T. ) ;
#619 = CARTESIAN_POINT ( 'NONE',  ( 0.000000000000000000, -27.07404830566974141, 4.815694066514342175 ) ) ;
#620 = LINE ( 'NONE', #11105, #13677 ) ;
#621 = CIRCLE ( 'NONE', #16136, 92.50100000000001899 ) ;
#622 = ORIENTED_EDGE ( 'NONE', *, *, #14710, .F. ) ;
#623 = DIRECTION ( 'NONE',  ( 1.000000000000000000, -0.000000000000000000, -0.000000000000000000 ) ) ;
#624 = DIRECTION ( 'NONE',  ( -0.000000000000000000, 0.000000000000000000, 1.000000000000000000 ) ) ;
#625 = CARTESIAN_POINT ( 'NONE',  ( 0.000000000000000000, 41.21966518005955038, 82.80926399530301296 ) ) ;
#626 = CARTESIAN_POINT ( 'NONE',  ( 7.440711023145602176, 0.000000000000000000, 0.000000000000000000 ) ) ;
#627 = DIRECTION ( 'NONE',  ( -1.000000000000000000, -0.000000000000000000, 0.000000000000000000 ) ) ;
#628 = VERTEX_POINT ( 'NONE', #13806 ) ;
#629 = CARTESIAN_POINT ( 'NONE',  ( 10.00000000000000000, 62.44821182181184582, -68.23969402963440700 ) ) ;
#630 = CIRCLE ( 'NONE', #2393, 44.99999999999999289 ) ;
#631 = AXIS2_PLACEMENT_3D ( 'NONE', #19053, #12308, #16964 ) ;
#632 = DIRECTION ( 'NONE',  ( 0.000000000000000000, -0.8660254037844327124, -0.5000000000000103251 ) ) ;
#633 = CIRCLE ( 'NONE', #5574, 11.99999999999999645 ) ;
#634 = CARTESIAN_POINT ( 'NONE',  ( 10.00000000000000000, 0.000000000000000000, 0.000000000000000000 ) ) ;
#635 = EDGE_LOOP ( 'NONE', ( #2174, #21660, #4771, #5388 ) ) ;
#636 = DIRECTION ( 'NONE',  ( 0.000000000000000000, 0.000000000000000000, 1.000000000000000000 ) ) ;
#637 = ORIENTED_EDGE ( 'NONE', *, *, #6937, .T. ) ;
#638 = CYLINDRICAL_SURFACE ( 'NONE', #2415, 45.00000000000000000 ) ;
#639 = ORIENTED_EDGE ( 'NONE', *, *, #10676, .T. ) ;
#640 = ORIENTED_EDGE ( 'NONE', *, *, #862, .T. ) ;
#641 = EDGE_CURVE ( 'NONE', #13683, #10766, #5390, .T. ) ;
#642 = ORIENTED_EDGE ( 'NONE', *, *, #6404, .T. ) ;
#643 = CARTESIAN_POINT ( 'NONE',  ( -10.00000000000000000, 0.000000000000000000, 0.000000000000000000 ) ) ;
#644 = ORIENTED_EDGE ( 'NONE', *, *, #3566, .T. ) ;
#645 = FACE_OUTER_BOUND ( 'NONE', #12452, .T. ) ;
#646 = AXIS2_PLACEMENT_3D ( 'NONE', #7957, #770, #14364 ) ;
#647 = DIRECTION ( 'NONE',  ( 1.000000000000000000, 0.000000000000000000, 0.000000000000000000 ) ) ;
#648 = DIRECTION ( 'NONE',  ( 0.000000000000000000, 0.000000000000000000, 1.000000000000000000 ) ) ;
#649 = VECTOR ( 'NONE', #1759, 1000.000000000000000 ) ;
#650 = AXIS2_PLACEMENT_3D ( 'NONE', #3327, #16813, #1788 ) ;
#651 = AXIS2_PLACEMENT_3D ( 'NONE', #18135, #14591, #2989 ) ;
#652 = DIRECTION ( 'NONE',  ( -1.000000000000000000, 0.000000000000000000, 0.000000000000000000 ) ) ;
#653 = ADVANCED_FACE ( 'NONE', ( #15782 ), #20449, .F. ) ;
#654 = FACE_OUTER_BOUND ( 'NONE', #10649, .T. ) ;
#655 = CYLINDRICAL_SURFACE ( 'NONE', #14717, 88.00000000000000000 ) ;
#656 = DIRECTION ( 'NONE',  ( 0.000000000000000000, 0.000000000000000000, -1.000000000000000000 ) ) ;
#657 = DIRECTION ( 'NONE',  ( -1.000000000000000000, 0.000000000000000000, 0.000000000000000000 ) ) ;
#658 = DIRECTION ( 'NONE',  ( -1.000000000000000000, 0.000000000000000000, 0.000000000000000000 ) ) ;
#659 = VERTEX_POINT ( 'NONE', #12137 ) ;
#660 = DIRECTION ( 'NONE',  ( -0.000000000000000000, -0.000000000000000000, -1.000000000000000000 ) ) ;
#661 = AXIS2_PLACEMENT_3D ( 'NONE', #13901, #18996, #17342 ) ;
#662 = ORIENTED_EDGE ( 'NONE', *, *, #19083, .F. ) ;
#663 = AXIS2_PLACEMENT_3D ( 'NONE', #18207, #3060, #9786 ) ;
#664 = ORIENTED_EDGE ( 'NONE', *, *, #11903, .T. ) ;
#665 = CIRCLE ( 'NONE', #2431, 92.50100000000000477 ) ;
#666 = AXIS2_PLACEMENT_3D ( 'NONE', #6861, #10168, #5524 ) ;
#667 = VERTEX_POINT ( 'NONE', #18888 ) ;
#668 = FACE_BOUND ( 'NONE', #13244, .T. ) ;
#669 = ORIENTED_EDGE ( 'NONE', *, *, #11797, .T. ) ;
#670 = EDGE_CURVE ( 'NONE', #9397, #13601, #10805, .T. ) ;
#671 = ADVANCED_FACE ( 'NONE', ( #17558 ), #2098, .T. ) ;
#672 = EDGE_LOOP ( 'NONE', ( #10904, #6762, #21714, #12996 ) ) ;
#673 = ORIENTED_EDGE ( 'NONE', *, *, #21444, .T. ) ;
#674 = CARTESIAN_POINT ( 'NONE',  ( 0.000000000000000000, 100.0000000000000000, 0.000000000000000000 ) ) ;
#675 = EDGE_CURVE ( 'NONE', #17526, #5244, #19164, .T. ) ;
#676 = ORIENTED_EDGE ( 'NONE', *, *, #17682, .F. ) ;
#677 = FACE_OUTER_BOUND ( 'NONE', #2204, .T. ) ;
#678 = CARTESIAN_POINT ( 'NONE',  ( 10.00000000000000000, 0.000000000000000000, 0.000000000000000000 ) ) ;
#679 = AXIS2_PLACEMENT_3D ( 'NONE', #20194, #6619, #4621 ) ;
#680 = DIRECTION ( 'NONE',  ( 0.000000000000000000, -0.4067366430757888285, -0.9135454576426059736 ) ) ;
#681 = CYLINDRICAL_SURFACE ( 'NONE', #11395, 11.99999999999999822 ) ;
#682 = CARTESIAN_POINT ( 'NONE',  ( 10.00000000000000000, 0.000000000000000000, 0.000000000000000000 ) ) ;
#683 = MECHANICAL_DESIGN_GEOMETRIC_PRESENTATION_REPRESENTATION (  '', ( #2802 ), #19738 ) ;
#684 = AXIS2_PLACEMENT_3D ( 'NONE', #20100, #1853, #13565 ) ;
#685 = FACE_OUTER_BOUND ( 'NONE', #14334, .T. ) ;
#686 = DIRECTION ( 'NONE',  ( -1.000000000000000000, 0.000000000000000000, 0.000000000000000000 ) ) ;
#687 = EDGE_CURVE ( 'NONE', #13715, #20567, #2193, .T. ) ;
#688 = DIRECTION ( 'NONE',  ( -1.000000000000000000, 0.000000000000000000, -0.000000000000000000 ) ) ;
#689 = ORIENTED_EDGE ( 'NONE', *, *, #10298, .T. ) ;
#690 = EDGE_CURVE ( 'NONE', #13273, #6116, #14924, .T. ) ;
#691 = LINE ( 'NONE', #12093, #15370 ) ;
#692 = CYLINDRICAL_SURFACE ( 'NONE', #12976, 27.49900000000000233 ) ;
#693 = DIRECTION ( 'NONE',  ( 1.000000000000000000, 0.000000000000000000, 0.000000000000000000 ) ) ;
#694 = ADVANCED_FACE ( 'NONE', ( #3962 ), #7170, .T. ) ;
#695 = EDGE_LOOP ( 'NONE', ( #21049, #1674, #16074, #3574 ) ) ;
#696 = ADVANCED_FACE ( 'NONE', ( #2956 ), #11142, .T. ) ;
#697 = AXIS2_PLACEMENT_3D ( 'NONE', #16951, #8544, #9755 ) ;
#698 = DIRECTION ( 'NONE',  ( 0.000000000000000000, 0.9945218953682737340, -0.1045284632676503622 ) ) ;
#699 = AXIS2_PLACEMENT_3D ( 'NONE', #2722, #7806, #14768 ) ;
#700 = ORIENTED_EDGE ( 'NONE', *, *, #9307, .F. ) ;
#701 = CARTESIAN_POINT ( 'NONE',  ( 0.000000000000000000, 0.000000000000000000, 0.000000000000000000 ) ) ;
#702 = EDGE_CURVE ( 'NONE', #1080, #2507, #16323, .T. ) ;
#703 = ORIENTED_EDGE ( 'NONE', *, *, #1678, .T. ) ;
#704 = EDGE_LOOP ( 'NONE', ( #7336, #749, #17679, #6492 ) ) ;
#705 = DIRECTION ( 'NONE',  ( -1.000000000000000000, 0.000000000000000000, -0.000000000000000000 ) ) ;
#706 = DIRECTION ( 'NONE',  ( -1.000000000000000000, 0.000000000000000000, -0.000000000000000000 ) ) ;
#707 = DIRECTION ( 'NONE',  ( 0.000000000000000000, 0.000000000000000000, 1.000000000000000000 ) ) ;
#708 = DIRECTION ( 'NONE',  ( 0.000000000000000000, 0.000000000000000000, -1.000000000000000000 ) ) ;
#709 = DIRECTION ( 'NONE',  ( 1.000000000000000000, 0.000000000000000000, 0.000000000000000000 ) ) ;
#710 = DIRECTION ( 'NONE',  ( -1.000000000000000000, 0.000000000000000000, 0.000000000000000000 ) ) ;
#711 = DIRECTION ( 'NONE',  ( 1.000000000000000000, 0.000000000000000000, 0.000000000000000000 ) ) ;
#712 = EDGE_CURVE ( 'NONE', #14549, #21211, #470, .T. ) ;
#713 = DIRECTION ( 'NONE',  ( 0.000000000000000000, 0.000000000000000000, 1.000000000000000000 ) ) ;
#714 = AXIS2_PLACEMENT_3D ( 'NONE', #18039, #9610, #5889 ) ;
#715 = VERTEX_POINT ( 'NONE', #17891 ) ;
#716 = EDGE_CURVE ( 'NONE', #7135, #13798, #8224, .T. ) ;
#717 = CYLINDRICAL_SURFACE ( 'NONE', #8680, 45.00000000000000000 ) ;
#718 = EDGE_LOOP ( 'NONE', ( #1372, #13579, #6111, #12415 ) ) ;
#719 = ADVANCED_FACE ( 'NONE', ( #7822 ), #1191, .T. ) ;
#720 = DIRECTION ( 'NONE',  ( 0.000000000000000000, 0.000000000000000000, 1.000000000000000000 ) ) ;
#721 = ORIENTED_EDGE ( 'NONE', *, *, #9312, .F. ) ;
#722 = CARTESIAN_POINT ( 'NONE',  ( 0.000000000000000000, 12.90135963484081216, 87.04915231966650424 ) ) ;
#723 = FACE_OUTER_BOUND ( 'NONE', #4694, .T. ) ;
#724 = ORIENTED_EDGE ( 'NONE', *, *, #1221, .T. ) ;
#725 =( NAMED_UNIT ( * ) PLANE_ANGLE_UNIT ( ) SI_UNIT ( $, .RADIAN. ) );
#726 = ORIENTED_EDGE ( 'NONE', *, *, #7475, .T. ) ;
#727 = ADVANCED_FACE ( 'NONE', ( #14346 ), #11021, .F. ) ;
#728 = ORIENTED_EDGE ( 'NONE', *, *, #6190, .F. ) ;
#729 = ORIENTED_EDGE ( 'NONE', *, *, #19205, .F. ) ;
#730 = AXIS2_PLACEMENT_3D ( 'NONE', #4831, #4390, #11574 ) ;
#731 = LINE ( 'NONE', #12221, #17426 ) ;
#732 = LINE ( 'NONE', #19288, #5569 ) ;
#733 = VERTEX_POINT ( 'NONE', #18005 ) ;
#734 = CARTESIAN_POINT ( 'NONE',  ( 0.000000000000000000, 46.89573839703275127, 79.73220629831503459 ) ) ;
#735 = DIRECTION ( 'NONE',  ( 1.000000000000000000, -0.000000000000000000, -0.000000000000000000 ) ) ;
#736 = CYLINDRICAL_SURFACE ( 'NONE', #5140, 27.49900000000000233 ) ;
#737 = CARTESIAN_POINT ( 'NONE',  ( 10.00000000000000000, 41.89587599971545018, 77.38692120905484728 ) ) ;
#738 = DIRECTION ( 'NONE',  ( 0.000000000000000000, 0.000000000000000000, 1.000000000000000000 ) ) ;
#739 = VERTEX_POINT ( 'NONE', #14558 ) ;
#740 = DIRECTION ( 'NONE',  ( 0.000000000000000000, 0.000000000000000000, 1.000000000000000000 ) ) ;
#741 = DIRECTION ( 'NONE',  ( 0.000000000000000000, 0.000000000000000000, 1.000000000000000000 ) ) ;
#742 = EDGE_CURVE ( 'NONE', #12477, #5806, #14229, .T. ) ;
#743 = DIRECTION ( 'NONE',  ( 0.000000000000000000, 0.000000000000000000, 1.000000000000000000 ) ) ;
#744 = EDGE_LOOP ( 'NONE', ( #351, #1727, #7139, #729 ) ) ;
#745 = CARTESIAN_POINT ( 'NONE',  ( -1.200000000000000844, 6.887500000000022382, 0.000000000000000000 ) ) ;
#746 = ORIENTED_EDGE ( 'NONE', *, *, #14200, .F. ) ;
#747 = FACE_OUTER_BOUND ( 'NONE', #17905, .T. ) ;
#748 = ORIENTED_EDGE ( 'NONE', *, *, #2986, .F. ) ;
#749 = ORIENTED_EDGE ( 'NONE', *, *, #6495, .F. ) ;
#750 = VERTEX_POINT ( 'NONE', #21197 ) ;
#751 = DIRECTION ( 'NONE',  ( 0.000000000000000000, 0.9945218953682729568, 0.1045284632676569958 ) ) ;
#752 = VERTEX_POINT ( 'NONE', #9469 ) ;
#753 = CYLINDRICAL_SURFACE ( 'NONE', #328, 120.0000000000000426 ) ;
#754 = DIRECTION ( 'NONE',  ( 1.000000000000000000, 0.000000000000000000, -0.000000000000000000 ) ) ;
#755 = DIRECTION ( 'NONE',  ( 1.000000000000000000, -0.000000000000000000, -0.000000000000000000 ) ) ;
#756 = AXIS2_PLACEMENT_3D ( 'NONE', #591, #2676, #7985 ) ;
#757 = DIRECTION ( 'NONE',  ( 0.000000000000000000, 0.5299192642332060110, -0.8480480961564252906 ) ) ;
#758 = CARTESIAN_POINT ( 'NONE',  ( 10.00000000000000000, 0.000000000000000000, 0.000000000000000000 ) ) ;
#759 = CARTESIAN_POINT ( 'NONE',  ( 0.000000000000000000, -12.94633825542284100, 24.26081875733330051 ) ) ;
#760 = CARTESIAN_POINT ( 'NONE',  ( -10.00000000000000888, 0.000000000000000000, 0.000000000000000000 ) ) ;
#761 = DIRECTION ( 'NONE',  ( -1.000000000000000000, -0.000000000000000000, -0.000000000000000000 ) ) ;
#762 = DIRECTION ( 'NONE',  ( 0.000000000000000000, 0.000000000000000000, 1.000000000000000000 ) ) ;
#763 = DIRECTION ( 'NONE',  ( 0.000000000000000000, 0.000000000000000000, -1.000000000000000000 ) ) ;
#764 = ORIENTED_EDGE ( 'NONE', *, *, #2482, .F. ) ;
#765 = AXIS2_PLACEMENT_3D ( 'NONE', #409, #2389, #9126 ) ;
#766 = EDGE_LOOP ( 'NONE', ( #18980, #17981, #8903, #8482, #6986, #6402, #13820, #2183 ) ) ;
#767 = ORIENTED_EDGE ( 'NONE', *, *, #6366, .T. ) ;
#768 = ORIENTED_EDGE ( 'NONE', *, *, #15411, .F. ) ;
#769 = VERTEX_POINT ( 'NONE', #21088 ) ;
#770 = DIRECTION ( 'NONE',  ( 1.000000000000000000, 0.000000000000000000, 0.000000000000000000 ) ) ;
#771 = VERTEX_POINT ( 'NONE', #861 ) ;
#772 = DIRECTION ( 'NONE',  ( 0.000000000000000000, 0.000000000000000000, -1.000000000000000000 ) ) ;
#773 = DIRECTION ( 'NONE',  ( 0.000000000000000000, 0.000000000000000000, 1.000000000000000000 ) ) ;
#774 = APPLICATION_CONTEXT ( 'automotive_design' ) ;
#775 = CARTESIAN_POINT ( 'NONE',  ( -5.000000000000000000, 8.660254037844385522, 15.00000000000000000 ) ) ;
#776 = CARTESIAN_POINT ( 'NONE',  ( 0.000000000000000000, 0.000000000000000000, 0.000000000000000000 ) ) ;
#777 = LINE ( 'NONE', #19128, #4471 ) ;
#778 = CARTESIAN_POINT ( 'NONE',  ( 10.00000000000000000, 19.07277123396568896, -19.80970465344728737 ) ) ;
#779 = DIRECTION ( 'NONE',  ( 1.000000000000000000, 0.000000000000000000, 0.000000000000000000 ) ) ;
#780 = CYLINDRICAL_SURFACE ( 'NONE', #12998, 10.49999999999999822 ) ;
#781 = AXIS2_PLACEMENT_3D ( 'NONE', #11638, #6451, #15157 ) ;
#782 = EDGE_CURVE ( 'NONE', #11100, #20998, #1173, .T. ) ;
#783 = VERTEX_POINT ( 'NONE', #9569 ) ;
#784 = DIRECTION ( 'NONE',  ( -1.000000000000000000, 0.000000000000000000, -0.000000000000000000 ) ) ;
#785 = EDGE_CURVE ( 'NONE', #13297, #18504, #11406, .T. ) ;
#786 = AXIS2_PLACEMENT_3D ( 'NONE', #20099, #4960, #11696 ) ;
#787 = CARTESIAN_POINT ( 'NONE',  ( 0.000000000000000000, 0.000000000000000000, 25.00000000000000000 ) ) ;
#788 = CARTESIAN_POINT ( 'NONE',  ( 0.000000000000000000, 0.000000000000000000, 0.000000000000000000 ) ) ;
#789 = ORIENTED_EDGE ( 'NONE', *, *, #14633, .F. ) ;
#790 = DIRECTION ( 'NONE',  ( -0.000000000000000000, -0.000000000000000000, -1.000000000000000000 ) ) ;
#791 = VERTEX_POINT ( 'NONE', #5849 ) ;
#792 = CARTESIAN_POINT ( 'NONE',  ( 0.000000000000000000, 0.000000000000000000, 0.000000000000000000 ) ) ;
#793 = ADVANCED_FACE ( 'NONE', ( #7721 ), #12574, .T. ) ;
#794 = CARTESIAN_POINT ( 'NONE',  ( 0.000000000000000000, -77.39385041987125646, -35.28996114464684553 ) ) ;
#795 = CIRCLE ( 'NONE', #461, 92.50100000000000477 ) ;
#796 = ORIENTED_EDGE ( 'NONE', *, *, #7154, .F. ) ;
#797 = VERTEX_POINT ( 'NONE', #5957 ) ;
#798 = LINE ( 'NONE', #17288, #11093 ) ;
#799 = CARTESIAN_POINT ( 'NONE',  ( 0.000000000000000000, -21.65267340503189430, -89.93106657554454841 ) ) ;
#800 = VECTOR ( 'NONE', #14018, 1000.000000000000000 ) ;
#801 = LINE ( 'NONE', #17290, #19926 ) ;
#802 = CARTESIAN_POINT ( 'NONE',  ( -10.00000000000002309, 0.000000000000000000, -118.9000000000000199 ) ) ;
#803 = DIRECTION ( 'NONE',  ( 1.000000000000000000, 0.000000000000000000, 0.000000000000000000 ) ) ;
#804 = DIRECTION ( 'NONE',  ( -1.000000000000000000, -0.000000000000000000, -0.000000000000000000 ) ) ;
#805 = FACE_OUTER_BOUND ( 'NONE', #14332, .T. ) ;
#806 = DIRECTION ( 'NONE',  ( -1.000000000000000000, 0.000000000000000000, 0.000000000000000000 ) ) ;
#807 = FACE_OUTER_BOUND ( 'NONE', #17843, .T. ) ;
#808 = EDGE_CURVE ( 'NONE', #1381, #2463, #1520, .T. ) ;
#809 = CIRCLE ( 'NONE', #16569, 44.99999999999999289 ) ;
#810 = ADVANCED_FACE ( 'NONE', ( #19317 ), #6296, .T. ) ;
#811 = EDGE_CURVE ( 'NONE', #9001, #20936, #12797, .T. ) ;
#812 = ORIENTED_EDGE ( 'NONE', *, *, #20256, .F. ) ;
#813 = DIRECTION ( 'NONE',  ( -1.000000000000000000, 0.000000000000000000, 0.000000000000000000 ) ) ;
#814 = ADVANCED_FACE ( 'NONE', ( #4516 ), #18101, .F. ) ;
#815 = AXIS2_PLACEMENT_3D ( 'NONE', #14347, #14231, #7936 ) ;
#816 = EDGE_LOOP ( 'NONE', ( #4202, #19739, #5033, #17926 ) ) ;
#817 = CARTESIAN_POINT ( 'NONE',  ( 0.000000000000000000, 27.82509854686817263, -4.525913221810857756 ) ) ;
#818 = ORIENTED_EDGE ( 'NONE', *, *, #17741, .T. ) ;
#819 = VECTOR ( 'NONE', #6483, 1000.000000000000000 ) ;
#820 = CARTESIAN_POINT ( 'NONE',  ( 10.00000000000000000, 83.35585896458643163, -16.94078559807864792 ) ) ;
#821 = ORIENTED_EDGE ( 'NONE', *, *, #4046, .T. ) ;
#822 = TOROIDAL_SURFACE ( 'NONE', #18833, 7.400000000000020783, 0.1000000000000001582 ) ;
#823 = FILL_AREA_STYLE_COLOUR ( '', #19105 ) ;
#824 = ADVANCED_FACE ( 'NONE', ( #16766 ), #1311, .F. ) ;
#825 = ORIENTED_EDGE ( 'NONE', *, *, #12856, .T. ) ;
#826 = VERTEX_POINT ( 'NONE', #6509 ) ;
#827 = VERTEX_POINT ( 'NONE', #10017 ) ;
#828 = FACE_OUTER_BOUND ( 'NONE', #3218, .T. ) ;
#829 = LINE ( 'NONE', #21054, #6628 ) ;
#830 = EDGE_LOOP ( 'NONE', ( #3498, #14260, #1454, #15635 ) ) ;
#831 = EDGE_CURVE ( 'NONE', #10390, #7164, #20196, .T. ) ;
#832 = CIRCLE ( 'NONE', #8597, 88.00000000000000000 ) ;
#833 = CARTESIAN_POINT ( 'NONE',  ( 0.000000000000000000, 0.000000000000000000, 0.000000000000000000 ) ) ;
#834 = CARTESIAN_POINT ( 'NONE',  ( 0.000000000000000000, 23.57863763525741874, -15.45211464167639548 ) ) ;
#835 = DIRECTION ( 'NONE',  ( -1.000000000000000000, -0.000000000000000000, -0.000000000000000000 ) ) ;
#836 = DIRECTION ( 'NONE',  ( 0.000000000000000000, 0.000000000000000000, 1.000000000000000000 ) ) ;
#837 = EDGE_CURVE ( 'NONE', #11042, #12235, #8052, .T. ) ;
#838 = DIRECTION ( 'NONE',  ( -1.000000000000000000, 0.000000000000000000, 0.000000000000000000 ) ) ;
#839 = VERTEX_POINT ( 'NONE', #13118 ) ;
#840 = AXIS2_PLACEMENT_3D ( 'NONE', #16403, #19825, #9765 ) ;
#841 = CARTESIAN_POINT ( 'NONE',  ( 10.00000000000000000, 0.000000000000000000, 0.000000000000000000 ) ) ;
#842 = EDGE_CURVE ( 'NONE', #7508, #15448, #1880, .T. ) ;
#843 = LINE ( 'NONE', #5831, #6195 ) ;
#844 = DIRECTION ( 'NONE',  ( 0.000000000000000000, -6.938893903907229167E-15, 1.000000000000000000 ) ) ;
#845 = VERTEX_POINT ( 'NONE', #3400 ) ;
#846 = CIRCLE ( 'NONE', #10371, 92.50100000000000477 ) ;
#847 = CARTESIAN_POINT ( 'NONE',  ( 10.00000000000000000, -24.89070495400792637, 84.40647372620493627 ) ) ;
#848 = ORIENTED_EDGE ( 'NONE', *, *, #1999, .T. ) ;
#849 = DIRECTION ( 'NONE',  ( 0.000000000000000000, 0.000000000000000000, 1.000000000000000000 ) ) ;
#850 = EDGE_LOOP ( 'NONE', ( #11771, #11484, #2762, #12556 ) ) ;
#851 = EDGE_CURVE ( 'NONE', #1324, #20085, #15279, .T. ) ;
#852 = CIRCLE ( 'NONE', #19198, 92.50099999999999056 ) ;
#853 = ORIENTED_EDGE ( 'NONE', *, *, #4633, .T. ) ;
#854 = ORIENTED_EDGE ( 'NONE', *, *, #12020, .F. ) ;
#855 = LINE ( 'NONE', #7604, #2634 ) ;
#856 = EDGE_CURVE ( 'NONE', #18401, #7456, #8589, .T. ) ;
#857 = CIRCLE ( 'NONE', #10034, 92.50100000000000477 ) ;
#858 = ORIENTED_EDGE ( 'NONE', *, *, #16652, .F. ) ;
#859 = LINE ( 'NONE', #15895, #13012 ) ;
#860 = CYLINDRICAL_SURFACE ( 'NONE', #6187, 44.99999999999999289 ) ;
#861 = CARTESIAN_POINT ( 'NONE',  ( 0.000000000000000000, -26.69209308833503513, -6.612652082459592684 ) ) ;
#862 = EDGE_CURVE ( 'NONE', #10755, #14140, #4705, .T. ) ;
#863 = LINE ( 'NONE', #3186, #9617 ) ;
#864 = EDGE_CURVE ( 'NONE', #15586, #17743, #13558, .T. ) ;
#865 = DIRECTION ( 'NONE',  ( -1.000000000000000000, 0.000000000000000000, -0.000000000000000000 ) ) ;
#866 = DIRECTION ( 'NONE',  ( -1.000000000000000000, 0.000000000000000000, 0.000000000000000000 ) ) ;
#867 = AXIS2_PLACEMENT_3D ( 'NONE', #14370, #5988, #12707 ) ;
#868 = CARTESIAN_POINT ( 'NONE',  ( 0.000000000000000000, 3.728035544477412255, -84.97818067823766341 ) ) ;
#869 = DIRECTION ( 'NONE',  ( 0.000000000000000000, 1.224646799147322392E-16, 1.000000000000000000 ) ) ;
#870 = CARTESIAN_POINT ( 'NONE',  ( 10.00000000000000000, 15.51843147776349063, 83.63233659819657362 ) ) ;
#871 = VECTOR ( 'NONE', #754, 1000.000000000000000 ) ;
#872 = CARTESIAN_POINT ( 'NONE',  ( 0.000000000000000000, -16.79755869217711250, 90.96305306542248559 ) ) ;
#873 = ORIENTED_EDGE ( 'NONE', *, *, #17135, .F. ) ;
#874 = VERTEX_POINT ( 'NONE', #18333 ) ;
#875 = ORIENTED_EDGE ( 'NONE', *, *, #21748, .F. ) ;
#876 = VECTOR ( 'NONE', #14562, 1000.000000000000000 ) ;
#877 = ORIENTED_EDGE ( 'NONE', *, *, #15846, .T. ) ;
#878 = AXIS2_PLACEMENT_3D ( 'NONE', #17750, #6154, #9440 ) ;
#879 = VERTEX_POINT ( 'NONE', #13337 ) ;
#880 = VECTOR ( 'NONE', #10189, 1000.000000000000000 ) ;
#881 = FACE_OUTER_BOUND ( 'NONE', #9645, .T. ) ;
#882 = EDGE_LOOP ( 'NONE', ( #18404, #3005, #16371, #10437 ) ) ;
#883 = CARTESIAN_POINT ( 'NONE',  ( 10.00000000000000000, -83.89484365856893078, -26.56417150043033359 ) ) ;
#884 = CARTESIAN_POINT ( 'NONE',  ( -7.600000000000001421, 0.000000000000000000, -105.0992000000000104 ) ) ;
#885 = AXIS2_PLACEMENT_3D ( 'NONE', #19974, #18332, #18752 ) ;
#886 = LINE ( 'NONE', #9268, #11719 ) ;
#887 = CARTESIAN_POINT ( 'NONE',  ( 10.00000000000000000, 0.000000000000000000, 0.000000000000000000 ) ) ;
#888 = FACE_OUTER_BOUND ( 'NONE', #15311, .T. ) ;
#889 = CARTESIAN_POINT ( 'NONE',  ( 7.395800000000001262, 0.000000000000000000, 0.000000000000000000 ) ) ;
#890 = CIRCLE ( 'NONE', #6565, 92.50099999999999056 ) ;
#891 = FACE_OUTER_BOUND ( 'NONE', #4555, .T. ) ;
#892 = DIRECTION ( 'NONE',  ( 1.000000000000000000, 0.000000000000000000, 0.000000000000000000 ) ) ;
#893 = DIRECTION ( 'NONE',  ( 0.000000000000000000, -0.1391731009600725710, 0.9902680687415692518 ) ) ;
#894 = AXIS2_PLACEMENT_3D ( 'NONE', #6128, #12845, #14176 ) ;
#895 = CIRCLE ( 'NONE', #21377, 3.000000000000000000 ) ;
#896 = ORIENTED_EDGE ( 'NONE', *, *, #17448, .T. ) ;
#897 = VECTOR ( 'NONE', #19140, 1000.000000000000000 ) ;
#898 = CIRCLE ( 'NONE', #16789, 44.99999999999998579 ) ;
#899 = DIRECTION ( 'NONE',  ( -1.000000000000000000, 0.000000000000000000, 0.000000000000000000 ) ) ;
#900 = DIRECTION ( 'NONE',  ( -1.000000000000000000, -0.000000000000000000, -0.000000000000000000 ) ) ;
#901 = CYLINDRICAL_SURFACE ( 'NONE', #8136, 44.99999999999999289 ) ;
#902 = ORIENTED_EDGE ( 'NONE', *, *, #2575, .T. ) ;
#903 = DIRECTION ( 'NONE',  ( 1.000000000000000000, 0.000000000000000000, 0.000000000000000000 ) ) ;
#904 = ORIENTED_EDGE ( 'NONE', *, *, #20980, .F. ) ;
#905 = ORIENTED_EDGE ( 'NONE', *, *, #5519, .T. ) ;
#906 = FACE_OUTER_BOUND ( 'NONE', #19726, .T. ) ;
#907 = ORIENTED_EDGE ( 'NONE', *, *, #5195, .T. ) ;
#908 = EDGE_CURVE ( 'NONE', #14453, #1080, #8374, .T. ) ;
#909 = CIRCLE ( 'NONE', #10107, 45.00000000000000000 ) ;
#910 = VERTEX_POINT ( 'NONE', #18216 ) ;
#911 = CARTESIAN_POINT ( 'NONE',  ( 10.00000000000000000, 56.05743251323954013, -67.83483072893743326 ) ) ;
#912 = AXIS2_PLACEMENT_3D ( 'NONE', #10757, #14292, #5583 ) ;
#913 = DIRECTION ( 'NONE',  ( 1.000000000000000000, -0.000000000000000000, 0.000000000000000000 ) ) ;
#914 = CIRCLE ( 'NONE', #11508, 44.99999999999999289 ) ;
#915 = DIRECTION ( 'NONE',  ( -1.000000000000000000, -0.000000000000000000, 0.000000000000000000 ) ) ;
#916 = CARTESIAN_POINT ( 'NONE',  ( 126.5000000000000000, 0.000000000000000000, -3.000000000000000000 ) ) ;
#917 = CARTESIAN_POINT ( 'NONE',  ( 10.00000000000000000, -72.53479564998751528, -44.42851404693431761 ) ) ;
#918 = CARTESIAN_POINT ( 'NONE',  ( 10.00000000000000000, 84.79630770241077187, 6.691460262316813790 ) ) ;
#919 = EDGE_CURVE ( 'NONE', #1655, #12268, #20311, .T. ) ;
#920 = CARTESIAN_POINT ( 'NONE',  ( 10.00000000000000000, 78.83848282823974785, -48.38314403117421847 ) ) ;
#921 = DIRECTION ( 'NONE',  ( 1.000000000000000000, 0.000000000000000000, 0.000000000000000000 ) ) ;
#922 = DIRECTION ( 'NONE',  ( -1.000000000000000000, -0.000000000000000000, 0.000000000000000000 ) ) ;
#923 = VERTEX_POINT ( 'NONE', #6621 ) ;
#924 = CARTESIAN_POINT ( 'NONE',  ( 5.000000000000000888, 30.61448696004452685, 9.314139153634330981 ) ) ;
#925 = ORIENTED_EDGE ( 'NONE', *, *, #3398, .F. ) ;
#926 = VECTOR ( 'NONE', #988, 1000.000000000000000 ) ;
#927 = CIRCLE ( 'NONE', #12927, 92.50099999999999056 ) ;
#928 = AXIS2_PLACEMENT_3D ( 'NONE', #10346, #4045, #12341 ) ;
#929 = FACE_OUTER_BOUND ( 'NONE', #18523, .T. ) ;
#930 = FILL_AREA_STYLE ('',( #16181 ) ) ;
#931 = CARTESIAN_POINT ( 'NONE',  ( 10.00000000000000000, -79.66702613806795341, 29.80527447819410369 ) ) ;
#932 = EDGE_LOOP ( 'NONE', ( #20151, #4122, #12521, #8046 ) ) ;
#933 = FILL_AREA_STYLE_COLOUR ( '', #3570 ) ;
#934 = ORIENTED_EDGE ( 'NONE', *, *, #20775, .T. ) ;
#935 = VERTEX_POINT ( 'NONE', #3072 ) ;
#936 = EDGE_CURVE ( 'NONE', #17111, #14755, #12097, .T. ) ;
#937 = EDGE_CURVE ( 'NONE', #11505, #5209, #18071, .T. ) ;
#938 = ORIENTED_EDGE ( 'NONE', *, *, #20300, .T. ) ;
#939 = EDGE_CURVE ( 'NONE', #6341, #4965, #11356, .T. ) ;
#940 = DIRECTION ( 'NONE',  ( 0.000000000000000000, 0.000000000000000000, 1.000000000000000000 ) ) ;
#941 = LINE ( 'NONE', #10997, #17560 ) ;
#942 = ORIENTED_EDGE ( 'NONE', *, *, #10497, .T. ) ;
#943 = CIRCLE ( 'NONE', #18950, 88.00000000000000000 ) ;
#944 = EDGE_CURVE ( 'NONE', #4641, #10985, #19860, .T. ) ;
#945 = CIRCLE ( 'NONE', #13292, 44.99999999999998579 ) ;
#946 = DIRECTION ( 'NONE',  ( 0.000000000000000000, -0.9993908270190960952, 0.03489949670249099800 ) ) ;
#947 = DIRECTION ( 'NONE',  ( -1.000000000000000000, 0.000000000000000000, 0.000000000000000000 ) ) ;
#948 = CIRCLE ( 'NONE', #1648, 0.1000000000000002554 ) ;
#949 = FACE_OUTER_BOUND ( 'NONE', #6336, .T. ) ;
#950 = DIRECTION ( 'NONE',  ( 0.000000000000000000, 0.000000000000000000, 1.000000000000000000 ) ) ;
#951 = AXIS2_PLACEMENT_3D ( 'NONE', #5313, #20121, #17241 ) ;
#952 = CARTESIAN_POINT ( 'NONE',  ( 10.00000000000000000, -90.32141448704695108, 19.96189084378191936 ) ) ;
#953 = ORIENTED_EDGE ( 'NONE', *, *, #4607, .T. ) ;
#954 = CYLINDRICAL_SURFACE ( 'NONE', #13043, 32.00000000000000000 ) ;
#955 = ADVANCED_FACE ( 'NONE', ( #21532 ), #6409, .F. ) ;
#956 = CARTESIAN_POINT ( 'NONE',  ( 0.000000000000000000, -82.02147376274702140, 42.76579056660835221 ) ) ;
#957 = EDGE_CURVE ( 'NONE', #20241, #20636, #5718, .T. ) ;
#958 = DIRECTION ( 'NONE',  ( 0.000000000000000000, 0.000000000000000000, 1.000000000000000000 ) ) ;
#959 = EDGE_LOOP ( 'NONE', ( #4249, #5076, #17336, #20807 ) ) ;
#960 = AXIS2_PLACEMENT_3D ( 'NONE', #12650, #6149, #14100 ) ;
#961 = DIRECTION ( 'NONE',  ( 0.000000000000000000, 0.000000000000000000, 1.000000000000000000 ) ) ;
#962 = AXIS2_PLACEMENT_3D ( 'NONE', #13792, #17107, #1971 ) ;
#963 = EDGE_LOOP ( 'NONE', ( #18501, #329, #19096, #19394 ) ) ;
#964 = CARTESIAN_POINT ( 'NONE',  ( 10.00000000000000000, 0.000000000000000000, 0.000000000000000000 ) ) ;
#965 = CIRCLE ( 'NONE', #3448, 88.00000000000000000 ) ;
#966 = VERTEX_POINT ( 'NONE', #10244 ) ;
#967 = EDGE_LOOP ( 'NONE', ( #4820, #9841, #7044, #8033 ) ) ;
#968 = EDGE_LOOP ( 'NONE', ( #5803, #6928, #18960, #21650 ) ) ;
#969 = EDGE_CURVE ( 'NONE', #1449, #453, #1838, .T. ) ;
#970 = CARTESIAN_POINT ( 'NONE',  ( 0.000000000000000000, -12.46320060045702860, -29.47318494484041196 ) ) ;
#971 = VERTEX_POINT ( 'NONE', #12335 ) ;
#972 = FACE_OUTER_BOUND ( 'NONE', #9390, .T. ) ;
#973 = EDGE_CURVE ( 'NONE', #839, #20292, #8403, .T. ) ;
#974 = FACE_OUTER_BOUND ( 'NONE', #9117, .T. ) ;
#975 = DIRECTION ( 'NONE',  ( 1.000000000000000000, 0.000000000000000000, 0.000000000000000000 ) ) ;
#976 = CARTESIAN_POINT ( 'NONE',  ( 0.000000000000000000, 17.64925110578583300, -86.21197095186326464 ) ) ;
#977 = AXIS2_PLACEMENT_3D ( 'NONE', #21570, #6448, #15046 ) ;
#978 = VECTOR ( 'NONE', #19817, 1000.000000000000000 ) ;
#979 = DIRECTION ( 'NONE',  ( 0.000000000000000000, 0.000000000000000000, -1.000000000000000000 ) ) ;
#980 = DIRECTION ( 'NONE',  ( 1.000000000000000000, 0.000000000000000000, 0.000000000000000000 ) ) ;
#981 = AXIS2_PLACEMENT_3D ( 'NONE', #13424, #14758, #11554 ) ;
#982 = AXIS2_PLACEMENT_3D ( 'NONE', #15495, #7108, #13941 ) ;
#983 = DIRECTION ( 'NONE',  ( 0.000000000000000000, 0.000000000000000000, 1.000000000000000000 ) ) ;
#984 = DIRECTION ( 'NONE',  ( 1.000000000000000000, 0.000000000000000000, 0.000000000000000000 ) ) ;
#985 = ADVANCED_FACE ( 'NONE', ( #2272 ), #16987, .T. ) ;
#986 = ADVANCED_FACE ( 'NONE', ( #8697 ), #2070, .F. ) ;
#987 = CIRCLE ( 'NONE', #16158, 32.00000000000000000 ) ;
#988 = DIRECTION ( 'NONE',  ( -1.000000000000000000, -0.000000000000000000, 0.000000000000000000 ) ) ;
#989 = ORIENTED_EDGE ( 'NONE', *, *, #9839, .T. ) ;
#990 = EDGE_LOOP ( 'NONE', ( #16974, #16725, #17713, #12754 ) ) ;
#991 = EDGE_CURVE ( 'NONE', #1185, #8085, #10864, .T. ) ;
#992 = EDGE_CURVE ( 'NONE', #10156, #6719, #16864, .T. ) ;
#993 = VERTEX_POINT ( 'NONE', #7052 ) ;
#994 = VECTOR ( 'NONE', #16575, 1000.000000000000000 ) ;
#995 = VECTOR ( 'NONE', #18944, 1000.000000000000000 ) ;
#996 = ORIENTED_EDGE ( 'NONE', *, *, #14739, .T. ) ;
#997 = CIRCLE ( 'NONE', #15090, 92.50100000000000477 ) ;
#998 = AXIS2_PLACEMENT_3D ( 'NONE', #20798, #10950, #12491 ) ;
#999 = ORIENTED_EDGE ( 'NONE', *, *, #7471, .T. ) ;
#1000 = CARTESIAN_POINT ( 'NONE',  ( 5.000000000000000000, 47.19205848891765243, 74.27590198428138990 ) ) ;
#1001 = ADVANCED_FACE ( 'NONE', ( #3935, #15432 ), #15758, .T. ) ;
#1002 = VERTEX_POINT ( 'NONE', #197 ) ;
#1003 = CARTESIAN_POINT ( 'NONE',  ( 0.000000000000000000, 87.92084725184948013, 3.731570516143270400 ) ) ;
#1004 = DIRECTION ( 'NONE',  ( 1.000000000000000000, -0.000000000000000000, -0.000000000000000000 ) ) ;
#1005 = DIRECTION ( 'NONE',  ( 0.000000000000000000, 0.000000000000000000, 1.000000000000000000 ) ) ;
#1006 = CARTESIAN_POINT ( 'NONE',  ( 10.00000000000000000, 0.000000000000000000, 0.000000000000000000 ) ) ;
#1007 = DIRECTION ( 'NONE',  ( 0.000000000000000000, 0.000000000000000000, 1.000000000000000000 ) ) ;
#1008 = DIRECTION ( 'NONE',  ( 0.000000000000000000, 0.000000000000000000, 1.000000000000000000 ) ) ;
#1009 = LINE ( 'NONE', #7756, #11856 ) ;
#1010 = CARTESIAN_POINT ( 'NONE',  ( 0.000000000000000000, 0.000000000000000000, 3.000000000000002665 ) ) ;
#1011 = CARTESIAN_POINT ( 'NONE',  ( 7.500000000000000000, 9.184850993605147944E-16, 3.000000000000000000 ) ) ;
#1012 = VECTOR ( 'NONE', #19204, 1000.000000000000000 ) ;
#1013 = AXIS2_PLACEMENT_3D ( 'NONE', #21234, #8600, #16784 ) ;
#1014 = CIRCLE ( 'NONE', #12642, 88.00000000000000000 ) ;
#1015 = ORIENTED_EDGE ( 'NONE', *, *, #12966, .F. ) ;
#1016 = AXIS2_PLACEMENT_3D ( 'NONE', #2312, #2525, #9046 ) ;
#1017 = DIRECTION ( 'NONE',  ( 0.000000000000000000, 0.000000000000000000, -1.000000000000000000 ) ) ;
#1018 = ORIENTED_EDGE ( 'NONE', *, *, #21788, .T. ) ;
#1019 = DIRECTION ( 'NONE',  ( 1.000000000000000000, 0.000000000000000000, 0.000000000000000000 ) ) ;
#1020 = DIRECTION ( 'NONE',  ( 1.000000000000000000, 0.000000000000000000, 0.000000000000000000 ) ) ;
#1021 = ORIENTED_EDGE ( 'NONE', *, *, #19486, .T. ) ;
#1022 = DIRECTION ( 'NONE',  ( -1.000000000000000000, 0.000000000000000000, 0.000000000000000000 ) ) ;
#1023 = EDGE_LOOP ( 'NONE', ( #18094, #13299, #11011, #7678 ) ) ;
#1024 = VERTEX_POINT ( 'NONE', #10668 ) ;
#1025 = AXIS2_PLACEMENT_3D ( 'NONE', #11902, #6831, #15939 ) ;
#1026 = CARTESIAN_POINT ( 'NONE',  ( 10.00000000000000000, -64.95266917914358373, 59.37298010462950515 ) ) ;
#1027 = EDGE_LOOP ( 'NONE', ( #1374, #15749, #17083, #5933 ) ) ;
#1028 = AXIS2_PLACEMENT_3D ( 'NONE', #2510, #17878, #9236 ) ;
#1029 = ORIENTED_EDGE ( 'NONE', *, *, #440, .T. ) ;
#1030 = DIRECTION ( 'NONE',  ( -1.000000000000000000, 0.000000000000000000, 0.000000000000000000 ) ) ;
#1031 = CIRCLE ( 'NONE', #19373, 27.49900000000000588 ) ;
#1032 = CIRCLE ( 'NONE', #15506, 44.99999999999998579 ) ;
#1033 = CARTESIAN_POINT ( 'NONE',  ( 0.000000000000000000, -51.18896083639317851, 71.57995730992162464 ) ) ;
#1034 = CYLINDRICAL_SURFACE ( 'NONE', #2287, 44.99999999999999289 ) ;
#1035 = CARTESIAN_POINT ( 'NONE',  ( 10.00000000000000000, 65.83713140174806711, -58.39068529131128571 ) ) ;
#1036 = FACE_OUTER_BOUND ( 'NONE', #4942, .T. ) ;
#1037 = DIRECTION ( 'NONE',  ( 1.000000000000000000, 0.000000000000000000, 0.000000000000000000 ) ) ;
#1038 = DIRECTION ( 'NONE',  ( -1.000000000000000000, -0.000000000000000000, 0.000000000000000000 ) ) ;
#1039 = CARTESIAN_POINT ( 'NONE',  ( 10.00000000000000000, -19.85071254963763465, -20.01672328094552356 ) ) ;
#1040 = DIRECTION ( 'NONE',  ( 0.000000000000000000, 0.000000000000000000, 1.000000000000000000 ) ) ;
#1041 = VERTEX_POINT ( 'NONE', #7374 ) ;
#1042 = FACE_OUTER_BOUND ( 'NONE', #8115, .T. ) ;
#1043 = CIRCLE ( 'NONE', #7406, 0.09999999999999939493 ) ;
#1044 = EDGE_CURVE ( 'NONE', #19647, #12067, #12628, .T. ) ;
#1045 = AXIS2_PLACEMENT_3D ( 'NONE', #3352, #1383, #4916 ) ;
#1046 = VERTEX_POINT ( 'NONE', #12111 ) ;
#1047 = AXIS2_PLACEMENT_3D ( 'NONE', #19279, #18850, #611 ) ;
#1048 = CIRCLE ( 'NONE', #12678, 44.99999999999999289 ) ;
#1049 = CARTESIAN_POINT ( 'NONE',  ( -1.200000000000006617, 6.873330160214519262E-16, 5.612499999999999822 ) ) ;
#1050 = CARTESIAN_POINT ( 'NONE',  ( -10.00000000000000000, 0.000000000000000000, 0.000000000000000000 ) ) ;
#1051 = ORIENTED_EDGE ( 'NONE', *, *, #20140, .T. ) ;
#1052 = EDGE_CURVE ( 'NONE', #10469, #1594, #17418, .T. ) ;
#1053 = SURFACE_SIDE_STYLE ('',( #9425 ) ) ;
#1054 = VERTEX_POINT ( 'NONE', #20843 ) ;
#1055 = ORIENTED_EDGE ( 'NONE', *, *, #8824, .T. ) ;
#1056 = VERTEX_POINT ( 'NONE', #6946 ) ;
#1057 = DIRECTION ( 'NONE',  ( 0.000000000000000000, -0.9271838545667832054, -0.3746065934159225619 ) ) ;
#1058 = LINE ( 'NONE', #12541, #19335 ) ;
#1059 = ORIENTED_EDGE ( 'NONE', *, *, #15255, .F. ) ;
#1060 = CARTESIAN_POINT ( 'NONE',  ( -10.00000000000000000, 0.000000000000000000, 0.000000000000000000 ) ) ;
#1061 = DIRECTION ( 'NONE',  ( -1.000000000000000000, -0.000000000000000000, -0.000000000000000000 ) ) ;
#1062 = CYLINDRICAL_SURFACE ( 'NONE', #1947, 92.50100000000000477 ) ;
#1063 = CIRCLE ( 'NONE', #11989, 32.00000000000000000 ) ;
#1064 = CARTESIAN_POINT ( 'NONE',  ( 0.000000000000000000, 0.000000000000000000, 0.000000000000000000 ) ) ;
#1065 = DIRECTION ( 'NONE',  ( 1.000000000000000000, 0.000000000000000000, 0.000000000000000000 ) ) ;
#1066 = VERTEX_POINT ( 'NONE', #3832 ) ;
#1067 = DIRECTION ( 'NONE',  ( -1.000000000000000000, 0.000000000000000000, 0.000000000000000000 ) ) ;
#1068 = DIRECTION ( 'NONE',  ( -1.000000000000000000, 0.000000000000000000, 0.000000000000000000 ) ) ;
#1069 = ADVANCED_FACE ( 'NONE', ( #13669 ), #5707, .T. ) ;
#1070 = ORIENTED_EDGE ( 'NONE', *, *, #10900, .F. ) ;
#1071 = CARTESIAN_POINT ( 'NONE',  ( 6.499999999999984901, 60.00000000000001421, -3.000000000000000000 ) ) ;
#1072 = ORIENTED_EDGE ( 'NONE', *, *, #21649, .T. ) ;
#1073 = CARTESIAN_POINT ( 'NONE',  ( 0.000000000000000000, 0.000000000000000000, 0.000000000000000000 ) ) ;
#1074 = DIRECTION ( 'NONE',  ( 1.000000000000000000, 0.000000000000000000, 0.000000000000000000 ) ) ;
#1075 = VERTEX_POINT ( 'NONE', #12011 ) ;
#1076 = FACE_OUTER_BOUND ( 'NONE', #15687, .T. ) ;
#1077 = ORIENTED_EDGE ( 'NONE', *, *, #16064, .F. ) ;
#1078 = ORIENTED_EDGE ( 'NONE', *, *, #3097, .T. ) ;
#1079 = DIRECTION ( 'NONE',  ( 0.000000000000000000, -5.396917480816734322E-15, -1.000000000000000000 ) ) ;
#1080 = VERTEX_POINT ( 'NONE', #13876 ) ;
#1081 = ADVANCED_FACE ( 'NONE', ( #10457 ), #1957, .F. ) ;
#1082 = CARTESIAN_POINT ( 'NONE',  ( 10.00000000000000000, 7.409634587003466777, -27.19958299168149907 ) ) ;
#1083 = CARTESIAN_POINT ( 'NONE',  ( 10.00000000000000000, 0.000000000000000000, 0.000000000000000000 ) ) ;
#1084 = DIRECTION ( 'NONE',  ( 1.000000000000000000, 0.000000000000000000, 0.000000000000000000 ) ) ;
#1085 = CARTESIAN_POINT ( 'NONE',  ( -90.00000000000000000, 0.000000000000000000, 0.000000000000000000 ) ) ;
#1086 = EDGE_CURVE ( 'NONE', #10454, #12130, #13989, .T. ) ;
#1087 = DIRECTION ( 'NONE',  ( 1.000000000000000000, 0.000000000000000000, 0.000000000000000000 ) ) ;
#1088 = CARTESIAN_POINT ( 'NONE',  ( 10.00000000000000000, 0.000000000000000000, 0.000000000000000000 ) ) ;
#1089 = VECTOR ( 'NONE', #5047, 1000.000000000000000 ) ;
#1090 = DIRECTION ( 'NONE',  ( 0.000000000000000000, -0.9945218953682722907, -0.1045284632676634767 ) ) ;
#1091 = CARTESIAN_POINT ( 'NONE',  ( 0.000000000000000000, 0.000000000000000000, 0.000000000000000000 ) ) ;
#1092 = ADVANCED_FACE ( 'NONE', ( #10571 ), #8896, .F. ) ;
#1093 = EDGE_CURVE ( 'NONE', #3248, #19526, #4523, .T. ) ;
#1094 = ADVANCED_FACE ( 'NONE', ( #10890 ), #9439, .F. ) ;
#1095 = FACE_OUTER_BOUND ( 'NONE', #12563, .T. ) ;
#1096 = VERTEX_POINT ( 'NONE', #21276 ) ;
#1097 = EDGE_CURVE ( 'NONE', #6661, #9836, #21450, .T. ) ;
#1098 = ORIENTED_EDGE ( 'NONE', *, *, #9059, .T. ) ;
#1099 = VERTEX_POINT ( 'NONE', #11111 ) ;
#1100 = ORIENTED_EDGE ( 'NONE', *, *, #14360, .T. ) ;
#1101 = STYLED_ITEM ( 'NONE', ( #19496 ), #2505 ) ;
#1102 = ORIENTED_EDGE ( 'NONE', *, *, #8383, .T. ) ;
#1103 = EDGE_CURVE ( 'NONE', #13440, #5078, #15091, .T. ) ;
#1104 = CARTESIAN_POINT ( 'NONE',  ( 10.00000000000000000, 1.959304526718168571, -27.42911093658673138 ) ) ;
#1105 = ORIENTED_EDGE ( 'NONE', *, *, #19818, .F. ) ;
#1106 = CYLINDRICAL_SURFACE ( 'NONE', #89, 5.000000000000000000 ) ;
#1107 = CARTESIAN_POINT ( 'NONE',  ( -140.0000507999999968, 0.000000000000000000, 3.000000000000000444 ) ) ;
#1108 = EDGE_CURVE ( 'NONE', #16260, #21189, #633, .T. ) ;
#1109 = DIRECTION ( 'NONE',  ( -1.000000000000000000, 0.000000000000000000, 0.000000000000000000 ) ) ;
#1110 = DIRECTION ( 'NONE',  ( -1.000000000000000000, 0.000000000000000000, 0.000000000000000000 ) ) ;
#1111 = CARTESIAN_POINT ( 'NONE',  ( 10.00000000000000000, 12.94633825542301153, -24.26081875733320814 ) ) ;
#1112 = EDGE_CURVE ( 'NONE', #13174, #7194, #7347, .T. ) ;
#1113 = CARTESIAN_POINT ( 'NONE',  ( -10.00000000000000000, 0.000000000000000000, 0.000000000000000000 ) ) ;
#1114 = CARTESIAN_POINT ( 'NONE',  ( 7.599999999999998757, 0.000000000000000000, -105.0992000000000104 ) ) ;
#1115 = DIRECTION ( 'NONE',  ( 0.000000000000000000, 0.000000000000000000, 1.000000000000000000 ) ) ;
#1116 = COLOUR_RGB ( '', 0.31764706, 0.68627451, 0.89019608) ;
#1117 = ORIENTED_EDGE ( 'NONE', *, *, #8904, .T. ) ;
#1118 = DIRECTION ( 'NONE',  ( -1.000000000000000000, -0.000000000000000000, -0.000000000000000000 ) ) ;
#1119 = EDGE_CURVE ( 'NONE', #6824, #5168, #17976, .T. ) ;
#1120 = VERTEX_POINT ( 'NONE', #17749 ) ;
#1122 = EDGE_CURVE ( 'NONE', #1840, #510, #2828, .T. ) ;
#1121 = AXIS2_PLACEMENT_3D ( 'NONE', #5058, #82, #8485 ) ;
#1123 = DIRECTION ( 'NONE',  ( -1.000000000000000000, 0.000000000000000000, -0.000000000000000000 ) ) ;
#1124 = DIRECTION ( 'NONE',  ( 0.000000000000000000, 0.000000000000000000, 1.000000000000000000 ) ) ;
#1125 = ORIENTED_EDGE ( 'NONE', *, *, #2337, .T. ) ;
#1126 = DIRECTION ( 'NONE',  ( 0.000000000000000000, 0.5877852522924688072, 0.8090169943749505599 ) ) ;
#1127 = VERTEX_POINT ( 'NONE', #4265 ) ;
#1128 = VERTEX_POINT ( 'NONE', #9123 ) ;
#1129 = CARTESIAN_POINT ( 'NONE',  ( 1.130367154297494105E-15, 1.499999999999999556, 4.057370503145720917E-16 ) ) ;
#1130 = DIRECTION ( 'NONE',  ( 1.000000000000000000, -0.000000000000000000, 0.000000000000000000 ) ) ;
#1131 = ORIENTED_EDGE ( 'NONE', *, *, #11671, .T. ) ;
#1132 = ORIENTED_EDGE ( 'NONE', *, *, #4715, .F. ) ;
#1133 = PRODUCT_DEFINITION_FORMATION_WITH_SPECIFIED_SOURCE ( 'ANY', '', #4726, .NOT_KNOWN. ) ;
#1134 = CARTESIAN_POINT ( 'NONE',  ( 5.000000000000002665, -17.64925110578526812, 86.21197095186339254 ) ) ;
#1135 = ADVANCED_FACE ( 'NONE', ( #2497 ), #9223, .F. ) ;
#1136 = DIRECTION ( 'NONE',  ( -1.000000000000000000, -0.000000000000000000, -0.000000000000000000 ) ) ;
#1137 = VECTOR ( 'NONE', #21789, 1000.000000000000000 ) ;
#1138 = DIRECTION ( 'NONE',  ( -1.000000000000000000, 0.000000000000000000, -0.000000000000000000 ) ) ;
#1139 = DIRECTION ( 'NONE',  ( 0.000000000000000000, 0.000000000000000000, 1.000000000000000000 ) ) ;
#1140 = DIRECTION ( 'NONE',  ( -1.000000000000000000, 0.000000000000000000, -0.000000000000000000 ) ) ;
#1141 = CYLINDRICAL_SURFACE ( 'NONE', #4749, 88.00000000000000000 ) ;
#1142 = ADVANCED_FACE ( 'NONE', ( #14644, #12759 ), #12545, .T. ) ;
#1143 = FACE_OUTER_BOUND ( 'NONE', #3471, .T. ) ;
#1144 = CARTESIAN_POINT ( 'NONE',  ( 10.00000000000000000, -23.57863763525709189, -15.45211464167688753 ) ) ;
#1145 = FACE_OUTER_BOUND ( 'NONE', #10184, .T. ) ;
#1146 = AXIS2_PLACEMENT_3D ( 'NONE', #6429, #8181, #19885 ) ;
#1147 = EDGE_LOOP ( 'NONE', ( #21730, #17643, #10337, #13826 ) ) ;
#1148 = AXIS2_PLACEMENT_3D ( 'NONE', #12342, #2173, #10349 ) ;
#1149 = DIRECTION ( 'NONE',  ( -1.000000000000000000, -0.000000000000000000, -0.000000000000000000 ) ) ;
#1150 = ORIENTED_EDGE ( 'NONE', *, *, #10525, .T. ) ;
#1151 = DIRECTION ( 'NONE',  ( -1.000000000000000000, -0.000000000000000000, -0.000000000000000000 ) ) ;
#1152 =( LENGTH_UNIT ( ) NAMED_UNIT ( * ) SI_UNIT ( .MILLI., .METRE. ) );
#1153 = MECHANICAL_DESIGN_GEOMETRIC_PRESENTATION_REPRESENTATION (  '', ( #14569 ), #20227 ) ;
#1154 = LINE ( 'NONE', #7564, #6347 ) ;
#1155 = ORIENTED_EDGE ( 'NONE', *, *, #4441, .F. ) ;
#1156 = EDGE_LOOP ( 'NONE', ( #622, #6943, #3985, #9583 ) ) ;
#1157 = CIRCLE ( 'NONE', #4338, 92.50100000000000477 ) ;
#1158 = AXIS2_PLACEMENT_3D ( 'NONE', #19000, #8927, #14126 ) ;
#1159 = ORIENTED_EDGE ( 'NONE', *, *, #13532, .T. ) ;
#1160 = ORIENTED_EDGE ( 'NONE', *, *, #10270, .F. ) ;
#1161 = CARTESIAN_POINT ( 'NONE',  ( 0.000000000000000000, 73.32282170386913833, -48.65967342042704757 ) ) ;
#1162 = DIRECTION ( 'NONE',  ( 1.000000000000000000, 0.000000000000000000, 0.000000000000000000 ) ) ;
#1163 = AXIS2_PLACEMENT_3D ( 'NONE', #13630, #11866, #16624 ) ;
#1164 = ORIENTED_EDGE ( 'NONE', *, *, #12479, .T. ) ;
#1165 = AXIS2_PLACEMENT_3D ( 'NONE', #5657, #19239, #3886 ) ;
#1166 = DIRECTION ( 'NONE',  ( 0.000000000000000000, -0.6946583704589887054, -0.7193398003386594075 ) ) ;
#1167 = DIRECTION ( 'NONE',  ( -1.000000000000000000, 0.000000000000000000, 0.000000000000000000 ) ) ;
#1168 = CARTESIAN_POINT ( 'NONE',  ( 0.000000000000000000, 81.97107881582226696, -22.71412948308482171 ) ) ;
#1169 = DIRECTION ( 'NONE',  ( -1.000000000000000000, 0.000000000000000000, 0.000000000000000000 ) ) ;
#1170 = DIRECTION ( 'NONE',  ( 0.000000000000000000, 0.000000000000000000, 1.000000000000000000 ) ) ;
#1171 = ORIENTED_EDGE ( 'NONE', *, *, #9708, .F. ) ;
#1172 = DIRECTION ( 'NONE',  ( 1.000000000000000000, 0.000000000000000000, 0.000000000000000000 ) ) ;
#1173 = CIRCLE ( 'NONE', #18468, 44.99999999999999289 ) ;
#1174 = CARTESIAN_POINT ( 'NONE',  ( 0.000000000000000000, -29.29369617358407396, -87.74003855418429509 ) ) ;
#1175 = ORIENTED_EDGE ( 'NONE', *, *, #10704, .T. ) ;
#1176 = AXIS2_PLACEMENT_3D ( 'NONE', #19936, #10094, #16839 ) ;
#1177 = FACE_OUTER_BOUND ( 'NONE', #14420, .T. ) ;
#1178 = VERTEX_POINT ( 'NONE', #17861 ) ;
#1179 = AXIS2_PLACEMENT_3D ( 'NONE', #8319, #21357, #1139 ) ;
#1180 = LINE ( 'NONE', #4712, #6697 ) ;
#1181 = DIRECTION ( 'NONE',  ( 1.000000000000000000, 0.000000000000000000, 0.000000000000000000 ) ) ;
#1182 = VERTEX_POINT ( 'NONE', #5928 ) ;
#1183 = DIRECTION ( 'NONE',  ( -1.000000000000000000, 0.000000000000000000, 0.000000000000000000 ) ) ;
#1184 = VERTEX_POINT ( 'NONE', #21173 ) ;
#1185 = VERTEX_POINT ( 'NONE', #2712 ) ;
#1186 = CARTESIAN_POINT ( 'NONE',  ( 10.00000000000000000, -31.88200538760791503, -2.745493118647322817 ) ) ;
#1187 = EDGE_LOOP ( 'NONE', ( #16962, #16925, #4808, #12317 ) ) ;
#1188 = CARTESIAN_POINT ( 'NONE',  ( 0.000000000000000000, 0.000000000000000000, 15.00000000000000000 ) ) ;
#1189 = CIRCLE ( 'NONE', #9291, 11.99999999999999822 ) ;
#1190 = CARTESIAN_POINT ( 'NONE',  ( 0.000000000000000000, -37.96946988134224910, 76.11510229470846411 ) ) ;
#1191 = CYLINDRICAL_SURFACE ( 'NONE', #9624, 32.00000000000000000 ) ;
#1192 = EDGE_CURVE ( 'NONE', #5691, #4328, #1346, .T. ) ;
#1193 = PRODUCT_DEFINITION_SHAPE ( 'NONE', 'NONE',  #21859 ) ;
#1194 = CARTESIAN_POINT ( 'NONE',  ( 10.00000000000000000, 52.34334029047875703, 76.26670130689501548 ) ) ;
#1195 = AXIS2_PLACEMENT_3D ( 'NONE', #3828, #2594, #4035 ) ;
#1196 = DIRECTION ( 'NONE',  ( 0.000000000000000000, 0.000000000000000000, 1.000000000000000000 ) ) ;
#1197 = DIRECTION ( 'NONE',  ( -1.000000000000000000, 0.000000000000000000, 0.000000000000000000 ) ) ;
#1198 = EDGE_CURVE ( 'NONE', #16573, #10108, #16519, .T. ) ;
#1199 = CARTESIAN_POINT ( 'NONE',  ( 0.000000000000000000, -27.40684453873977944, 16.51862198942000148 ) ) ;
#1200 = DIRECTION ( 'NONE',  ( -1.000000000000000000, 0.000000000000000000, -0.000000000000000000 ) ) ;
#1201 = VECTOR ( 'NONE', #7124, 1000.000000000000000 ) ;
#1202 = DIRECTION ( 'NONE',  ( 0.000000000000000000, 0.000000000000000000, 1.000000000000000000 ) ) ;
#1203 = CARTESIAN_POINT ( 'NONE',  ( 0.000000000000000000, 12.94633825542266869, 24.26081875733338933 ) ) ;
#1204 = APPLICATION_CONTEXT ( 'automotive_design' ) ;
#1205 = EDGE_CURVE ( 'NONE', #6716, #14855, #9432, .T. ) ;
#1206 = CIRCLE ( 'NONE', #19555, 27.49900000000000233 ) ;
#1207 = ORIENTED_EDGE ( 'NONE', *, *, #15551, .F. ) ;
#1208 = ORIENTED_EDGE ( 'NONE', *, *, #14309, .T. ) ;
#1209 = VECTOR ( 'NONE', #5021, 1000.000000000000000 ) ;
#1210 = EDGE_LOOP ( 'NONE', ( #20671, #21312, #12567, #637 ) ) ;
#1211 = ORIENTED_EDGE ( 'NONE', *, *, #13563, .T. ) ;
#1212 = EDGE_LOOP ( 'NONE', ( #11385, #19304, #21352, #17034, #4762, #16287, #21311, #7511 ) ) ;
#1213 = LINE ( 'NONE', #9932, #21124 ) ;
#1214 = CIRCLE ( 'NONE', #9305, 45.00000000000000000 ) ;
#1215 = ORIENTED_EDGE ( 'NONE', *, *, #21120, .T. ) ;
#1216 = DIRECTION ( 'NONE',  ( 0.000000000000000000, 0.000000000000000000, 1.000000000000000000 ) ) ;
#1217 = EDGE_CURVE ( 'NONE', #17002, #15753, #18642, .T. ) ;
#1218 = EDGE_CURVE ( 'NONE', #10690, #21676, #5822, .T. ) ;
#1219 = CARTESIAN_POINT ( 'NONE',  ( 10.00000000000000000, 90.32141448704707898, -19.96189084378132961 ) ) ;
#1220 = CIRCLE ( 'NONE', #19573, 5.000000000000000000 ) ;
#1221 = EDGE_CURVE ( 'NONE', #15501, #16339, #9099, .T. ) ;
#1222 = LINE ( 'NONE', #8076, #3271 ) ;
#1223 = DIRECTION ( 'NONE',  ( -1.000000000000000000, -0.000000000000000000, -0.000000000000000000 ) ) ;
#1224 = SURFACE_STYLE_USAGE ( .BOTH. , #18251 ) ;
#1225 = VECTOR ( 'NONE', #19473, 1000.000000000000000 ) ;
#1226 = CARTESIAN_POINT ( 'NONE',  ( -1.500000000000000000, 5.000000000000000000, 7.000000000000000000 ) ) ;
#1227 = DIRECTION ( 'NONE',  ( 0.000000000000000000, 0.000000000000000000, 1.000000000000000000 ) ) ;
#1228 = ORIENTED_EDGE ( 'NONE', *, *, #17732, .F. ) ;
#1229 = CARTESIAN_POINT ( 'NONE',  ( 0.000000000000000000, 0.000000000000000000, 0.000000000000000000 ) ) ;
#1230 = EDGE_CURVE ( 'NONE', #16156, #10882, #4696, .T. ) ;
#1231 = CIRCLE ( 'NONE', #1578, 44.99999999999999289 ) ;
#1232 = AXIS2_PLACEMENT_3D ( 'NONE', #16450, #15113, #10025 ) ;
#1233 = VERTEX_POINT ( 'NONE', #4596 ) ;
#1234 = ORIENTED_EDGE ( 'NONE', *, *, #1888, .F. ) ;
#1235 = DIRECTION ( 'NONE',  ( 0.000000000000000000, 1.000000000000000000, -1.224646799147353207E-16 ) ) ;
#1236 = EDGE_CURVE ( 'NONE', #7793, #21395, #2397, .T. ) ;
#1237 = VECTOR ( 'NONE', #13828, 1000.000000000000000 ) ;
#1238 = FACE_OUTER_BOUND ( 'NONE', #7650, .T. ) ;
#1239 = ORIENTED_EDGE ( 'NONE', *, *, #864, .F. ) ;
#1240 = DIRECTION ( 'NONE',  ( 0.000000000000000000, 0.000000000000000000, 1.000000000000000000 ) ) ;
#1241 = ORIENTED_EDGE ( 'NONE', *, *, #19219, .F. ) ;
#1242 = ORIENTED_EDGE ( 'NONE', *, *, #288, .F. ) ;
#1243 = CIRCLE ( 'NONE', #5123, 92.50100000000000477 ) ;
#1244 = DIRECTION ( 'NONE',  ( 0.000000000000000000, 0.000000000000000000, 1.000000000000000000 ) ) ;
#1245 = VERTEX_POINT ( 'NONE', #10102 ) ;
#1246 = VERTEX_POINT ( 'NONE', #16633 ) ;
#1247 = LINE ( 'NONE', #9295, #5456 ) ;
#1248 = DIRECTION ( 'NONE',  ( -1.000000000000000000, -0.000000000000000000, 0.000000000000000000 ) ) ;
#1249 = EDGE_CURVE ( 'NONE', #19371, #752, #11324, .T. ) ;
#1250 = CYLINDRICAL_SURFACE ( 'NONE', #527, 44.99999999999999289 ) ;
#1251 = CARTESIAN_POINT ( 'NONE',  ( 10.00000000000000000, 80.18694381077108346, 28.37681241246682973 ) ) ;
#1252 = CIRCLE ( 'NONE', #894, 88.00000000000000000 ) ;
#1253 = AXIS2_PLACEMENT_3D ( 'NONE', #9998, #13203, #16535 ) ;
#1254 = FILL_AREA_STYLE_COLOUR ( '', #5512 ) ;
#1255 = CARTESIAN_POINT ( 'NONE',  ( 0.000000000000000000, -14.53731623274945406, 23.34226719384900761 ) ) ;
#1256 = AXIS2_PLACEMENT_3D ( 'NONE', #11906, #8897, #17210 ) ;
#1257 = LINE ( 'NONE', #11412, #5780 ) ;
#1258 = DIRECTION ( 'NONE',  ( -1.000000000000000000, -0.000000000000000000, -0.000000000000000000 ) ) ;
#1260 = AXIS2_PLACEMENT_3D ( 'NONE', #11047, #7847, #16138 ) ;
#1259 = CARTESIAN_POINT ( 'NONE',  ( 10.00000000000000000, 0.000000000000000000, 0.000000000000000000 ) ) ;
#1261 = ORIENTED_EDGE ( 'NONE', *, *, #13381, .F. ) ;
#1262 = EDGE_CURVE ( 'NONE', #3326, #13846, #13699, .T. ) ;
#1263 = VERTEX_POINT ( 'NONE', #1394 ) ;
#1264 = CLOSED_SHELL ( 'NONE', ( #11800, #19951, #12732, #8634, #1598, #8913, #1358, #1778, #18719, #8874, #10287, #11609, #3169, #12589, #21642 ) ) ;
#1265 = EDGE_CURVE ( 'NONE', #12668, #14422, #17222, .T. ) ;
#1266 = AXIS2_PLACEMENT_3D ( 'NONE', #5002, #14839, #18487 ) ;
#1267 = DIRECTION ( 'NONE',  ( 0.000000000000000000, 1.233581138472396191E-14, -1.000000000000000000 ) ) ;
#1268 = DIRECTION ( 'NONE',  ( 0.000000000000000000, 0.000000000000000000, -1.000000000000000000 ) ) ;
#1269 = AXIS2_PLACEMENT_3D ( 'NONE', #17599, #10842, #5154 ) ;
#1270 = EDGE_CURVE ( 'NONE', #783, #19484, #3805, .T. ) ;
#1271 = LINE ( 'NONE', #16835, #19594 ) ;
#1272 = AXIS2_PLACEMENT_3D ( 'NONE', #2049, #5687, #15524 ) ;
#1273 = ORIENTED_EDGE ( 'NONE', *, *, #3235, .T. ) ;
#1274 = CIRCLE ( 'NONE', #16070, 126.5000000000000000 ) ;
#1275 = EDGE_CURVE ( 'NONE', #14473, #11791, #3046, .T. ) ;
#1276 = AXIS2_PLACEMENT_3D ( 'NONE', #7395, #19201, #751 ) ;
#1277 = ORIENTED_EDGE ( 'NONE', *, *, #3532, .T. ) ;
#1278 = ORIENTED_EDGE ( 'NONE', *, *, #13906, .T. ) ;
#1279 = ORIENTED_EDGE ( 'NONE', *, *, #11236, .T. ) ;
#1280 = FACE_OUTER_BOUND ( 'NONE', #14242, .T. ) ;
#1281 = PLANE ( 'NONE',  #4780 ) ;
#1282 = EDGE_LOOP ( 'NONE', ( #2209, #5838, #5505, #21179 ) ) ;
#1283 = DIRECTION ( 'NONE',  ( -1.000000000000000000, 0.000000000000000000, 0.000000000000000000 ) ) ;
#1284 = CYLINDRICAL_SURFACE ( 'NONE', #17187, 88.00000000000000000 ) ;
#1285 = LINE ( 'NONE', #6711, #21381 ) ;
#1286 = DIRECTION ( 'NONE',  ( 0.000000000000000000, 0.000000000000000000, 1.000000000000000000 ) ) ;
#1287 = LINE ( 'NONE', #19321, #4356 ) ;
#1288 = DIRECTION ( 'NONE',  ( 1.000000000000000000, -0.000000000000000000, -0.000000000000000000 ) ) ;
#1289 = UNCERTAINTY_MEASURE_WITH_UNIT (LENGTH_MEASURE( 1.000000000000000082E-05 ), #15116, 'distance_accuracy_value', 'NONE');
#1290 = CIRCLE ( 'NONE', #19275, 11.99999999999999822 ) ;
#1291 = ORIENTED_EDGE ( 'NONE', *, *, #19736, .T. ) ;
#1292 = CIRCLE ( 'NONE', #13628, 105.0992000000000104 ) ;
#1293 = DIRECTION ( 'NONE',  ( 0.000000000000000000, -1.000000000000000000, 0.000000000000000000 ) ) ;
#1294 = DIRECTION ( 'NONE',  ( 0.000000000000000000, 0.000000000000000000, -1.000000000000000000 ) ) ;
#1295 = VERTEX_POINT ( 'NONE', #21599 ) ;
#1296 = DIRECTION ( 'NONE',  ( 0.000000000000000000, -0.5877852522924632561, -0.8090169943749546677 ) ) ;
#1297 = VERTEX_POINT ( 'NONE', #11764 ) ;
#1298 = CARTESIAN_POINT ( 'NONE',  ( 0.000000000000000000, -19.29292659243987984, -25.53004080487782090 ) ) ;
#1299 = DIRECTION ( 'NONE',  ( 0.000000000000000000, -0.2079116908177468248, -0.9781476007338083534 ) ) ;
#1300 = ORIENTED_EDGE ( 'NONE', *, *, #1463, .T. ) ;
#1301 = DIRECTION ( 'NONE',  ( 1.000000000000000000, 0.000000000000000000, 0.000000000000000000 ) ) ;
#1302 = ORIENTED_EDGE ( 'NONE', *, *, #18247, .F. ) ;
#1303 = AXIS2_PLACEMENT_3D ( 'NONE', #16732, #1603, #18410 ) ;
#1304 = CIRCLE ( 'NONE', #7298, 6.728125000000023448 ) ;
#1305 = VERTEX_POINT ( 'NONE', #3154 ) ;
#1306 = CARTESIAN_POINT ( 'NONE',  ( 10.00000000000000000, -31.15801000616886896, 79.14775961996379294 ) ) ;
#1307 = AXIS2_PLACEMENT_3D ( 'NONE', #8958, #3991, #7524 ) ;
#1308 = VERTEX_POINT ( 'NONE', #2928 ) ;
#1309 = CARTESIAN_POINT ( 'NONE',  ( 5.000000000000000000, 23.37352460145283928, 21.85585385440887762 ) ) ;
#1310 = DIRECTION ( 'NONE',  ( -1.000000000000000000, 0.000000000000000000, 0.000000000000000000 ) ) ;
#1311 = CYLINDRICAL_SURFACE ( 'NONE', #20232, 44.99999999999999289 ) ;
#1312 = SURFACE_SIDE_STYLE ('',( #21739 ) ) ;
#1313 = CARTESIAN_POINT ( 'NONE',  ( 0.000000000000000000, -60.65655256511196569, -59.63197188857583342 ) ) ;
#1314 = FACE_OUTER_BOUND ( 'NONE', #13417, .T. ) ;
#1315 = CARTESIAN_POINT ( 'NONE',  ( 10.00000000000000000, 0.000000000000000000, 0.000000000000000000 ) ) ;
#1316 = FACE_OUTER_BOUND ( 'NONE', #17117, .T. ) ;
#1317 = CIRCLE ( 'NONE', #17186, 44.99999999999999289 ) ;
#1318 = DIRECTION ( 'NONE',  ( 0.000000000000000000, 0.000000000000000000, 1.000000000000000000 ) ) ;
#1319 = AXIS2_PLACEMENT_3D ( 'NONE', #12252, #2196, #5855 ) ;
#1320 = DIRECTION ( 'NONE',  ( 1.000000000000000000, 0.000000000000000000, 0.000000000000000000 ) ) ;
#1321 = ORIENTED_EDGE ( 'NONE', *, *, #7879, .T. ) ;
#1322 = EDGE_CURVE ( 'NONE', #10634, #19849, #13193, .T. ) ;
#1323 = ORIENTED_EDGE ( 'NONE', *, *, #12827, .F. ) ;
#1324 = VERTEX_POINT ( 'NONE', #16847 ) ;
#1325 = ORIENTED_EDGE ( 'NONE', *, *, #4026, .F. ) ;
#1326 = ADVANCED_FACE ( 'NONE', ( #8022, #19830 ), #14964, .F. ) ;
#1327 = EDGE_LOOP ( 'NONE', ( #11454, #5915, #8351, #1352 ) ) ;
#1328 = CARTESIAN_POINT ( 'NONE',  ( 10.00000000000000000, 79.66702613806732813, 29.80527447819576636 ) ) ;
#1329 = CIRCLE ( 'NONE', #19320, 44.99999999999999289 ) ;
#1330 = EDGE_LOOP ( 'NONE', ( #5862, #4662, #6873, #13438 ) ) ;
#1331 = CARTESIAN_POINT ( 'NONE',  ( 10.00000000000000000, -24.17932380791732427, 20.96092317126996818 ) ) ;
#1332 = CIRCLE ( 'NONE', #12251, 44.99999999999999289 ) ;
#1333 = AXIS2_PLACEMENT_3D ( 'NONE', #11197, #4347, #12847 ) ;
#1334 = DIRECTION ( 'NONE',  ( -1.000000000000000000, 0.000000000000000000, 0.000000000000000000 ) ) ;
#1335 = FACE_OUTER_BOUND ( 'NONE', #8331, .T. ) ;
#1336 = CARTESIAN_POINT ( 'NONE',  ( 0.000000000000000000, 0.000000000000000000, 0.000000000000000000 ) ) ;
#1337 = DIRECTION ( 'NONE',  ( -0.000000000000000000, -0.000000000000000000, -1.000000000000000000 ) ) ;
#1338 = DIRECTION ( 'NONE',  ( -1.000000000000000000, 0.000000000000000000, 0.000000000000000000 ) ) ;
#1339 = CYLINDRICAL_SURFACE ( 'NONE', #15828, 44.99999999999999289 ) ;
#1340 = EDGE_LOOP ( 'NONE', ( #11547, #938, #11995, #19443 ) ) ;
#1341 = DIRECTION ( 'NONE',  ( 0.000000000000000000, -0.8660254037844328234, -0.5000000000000101030 ) ) ;
#1342 = VECTOR ( 'NONE', #9120, 1000.000000000000000 ) ;
#1343 = ADVANCED_FACE ( 'NONE', ( #16525 ), #1284, .F. ) ;
#1344 = AXIS2_PLACEMENT_3D ( 'NONE', #6692, #13295, #13408 ) ;
#1345 = EDGE_CURVE ( 'NONE', #12967, #75, #20006, .T. ) ;
#1346 = CIRCLE ( 'NONE', #12978, 45.00000000000000000 ) ;
#1347 = VERTEX_POINT ( 'NONE', #18073 ) ;
#1348 = ORIENTED_EDGE ( 'NONE', *, *, #11032, .T. ) ;
#1349 = CARTESIAN_POINT ( 'NONE',  ( 0.000000000000000000, 0.000000000000000000, 88.00000000000000000 ) ) ;
#1350 = VERTEX_POINT ( 'NONE', #18511 ) ;
#1351 = CARTESIAN_POINT ( 'NONE',  ( -1.500000000000000000, 15.00000000000000000, 7.000000000000000000 ) ) ;
#1352 = ORIENTED_EDGE ( 'NONE', *, *, #16064, .T. ) ;
#1353 = ORIENTED_EDGE ( 'NONE', *, *, #11192, .F. ) ;
#1354 = CYLINDRICAL_SURFACE ( 'NONE', #21447, 5.612499999999999822 ) ;
#1355 = VERTEX_POINT ( 'NONE', #14863 ) ;
#1356 = CYLINDRICAL_SURFACE ( 'NONE', #13917, 120.0000000000000000 ) ;
#1357 = CARTESIAN_POINT ( 'NONE',  ( 10.00000000000000000, 0.000000000000000000, 0.000000000000000000 ) ) ;
#1358 = ADVANCED_FACE ( 'NONE', ( #13091 ), #3256, .T. ) ;
#1359 = AXIS2_PLACEMENT_3D ( 'NONE', #1891, #8630, #19665 ) ;
#1360 = CARTESIAN_POINT ( 'NONE',  ( 10.00000000000000000, 0.000000000000000000, 0.000000000000000000 ) ) ;
#1361 = DIRECTION ( 'NONE',  ( 0.000000000000000000, 0.000000000000000000, -1.000000000000000000 ) ) ;
#1362 = VECTOR ( 'NONE', #12240, 1000.000000000000000 ) ;
#1363 = DIRECTION ( 'NONE',  ( 0.000000000000000000, 0.9993908270190955401, 0.03489949670250439701 ) ) ;
#1364 = VECTOR ( 'NONE', #2984, 1000.000000000000000 ) ;
#1365 = CIRCLE ( 'NONE', #3821, 92.50099999999999056 ) ;
#1366 = DIRECTION ( 'NONE',  ( -1.000000000000000000, 0.000000000000000000, 0.000000000000000000 ) ) ;
#1367 = CIRCLE ( 'NONE', #13714, 44.99999999999999289 ) ;
#1368 = DIRECTION ( 'NONE',  ( -1.000000000000000000, 0.000000000000000000, 0.000000000000000000 ) ) ;
#1369 = EDGE_CURVE ( 'NONE', #20559, #15579, #20168, .T. ) ;
#1370 = CARTESIAN_POINT ( 'NONE',  ( 10.00000000000000000, 84.12297548659704205, 12.59025161327141618 ) ) ;
#1371 = DIRECTION ( 'NONE',  ( -1.000000000000000000, 0.000000000000000000, 0.000000000000000000 ) ) ;
#1372 = ORIENTED_EDGE ( 'NONE', *, *, #8112, .T. ) ;
#1373 = EDGE_CURVE ( 'NONE', #11931, #9160, #4118, .T. ) ;
#1374 = ORIENTED_EDGE ( 'NONE', *, *, #2299, .F. ) ;
#1375 = EDGE_CURVE ( 'NONE', #9371, #2869, #9653, .T. ) ;
#1376 = CIRCLE ( 'NONE', #324, 11.99999999999999822 ) ;
#1377 = CARTESIAN_POINT ( 'NONE',  ( 10.00000000000000000, 13.56333590714055326, -28.98337314858420299 ) ) ;
#1378 = CIRCLE ( 'NONE', #9127, 11.99999999999999822 ) ;
#1379 = EDGE_CURVE ( 'NONE', #12369, #21410, #2346, .T. ) ;
#1380 = CARTESIAN_POINT ( 'NONE',  ( 5.000000000000000000, 8.660254037844385522, 15.00000000000000000 ) ) ;
#1381 = VERTEX_POINT ( 'NONE', #6915 ) ;
#1382 = VECTOR ( 'NONE', #2261, 1000.000000000000000 ) ;
#1383 = DIRECTION ( 'NONE',  ( 1.000000000000000000, 0.000000000000000000, 0.000000000000000000 ) ) ;
#1384 = AXIS2_PLACEMENT_3D ( 'NONE', #16117, #984, #17782 ) ;
#1385 = ORIENTED_EDGE ( 'NONE', *, *, #16876, .F. ) ;
#1386 = EDGE_LOOP ( 'NONE', ( #19141, #2368, #1408, #10089 ) ) ;
#1387 = VERTEX_POINT ( 'NONE', #8559 ) ;
#1388 = VERTEX_POINT ( 'NONE', #18623 ) ;
#1389 = DIRECTION ( 'NONE',  ( 1.000000000000000000, 0.000000000000000000, 0.000000000000000000 ) ) ;
#1390 = DIRECTION ( 'NONE',  ( -1.000000000000000000, -0.000000000000000000, -0.000000000000000000 ) ) ;
#1391 = ORIENTED_EDGE ( 'NONE', *, *, #11842, .F. ) ;
#1392 = ADVANCED_FACE ( 'NONE', ( #5252 ), #1924, .F. ) ;
#1393 = DIRECTION ( 'NONE',  ( 0.000000000000000000, 0.000000000000000000, 1.000000000000000000 ) ) ;
#1394 = CARTESIAN_POINT ( 'NONE',  ( 0.000000000000000000, -87.92084725184945171, -3.731570516143874361 ) ) ;
#1395 = DIRECTION ( 'NONE',  ( 1.000000000000000000, 0.000000000000000000, 0.000000000000000000 ) ) ;
#1396 = EDGE_CURVE ( 'NONE', #18927, #10469, #10472, .T. ) ;
#1397 = DIRECTION ( 'NONE',  ( 0.000000000000000000, 0.7431448254773908024, 0.6691306063588620123 ) ) ;
#1398 = CARTESIAN_POINT ( 'NONE',  ( 10.00000000000000000, -10.41137886060169038, 91.91321010181843576 ) ) ;
#1399 = LINE ( 'NONE', #13197, #15906 ) ;
#1400 = CIRCLE ( 'NONE', #679, 88.00000000000000000 ) ;
#1401 = AXIS2_PLACEMENT_3D ( 'NONE', #14414, #15956, #9113 ) ;
#1402 = AXIS2_PLACEMENT_3D ( 'NONE', #12323, #20831, #10446 ) ;
#1403 = EDGE_LOOP ( 'NONE', ( #9580, #19229, #13619, #15952 ) ) ;
#1404 = CIRCLE ( 'NONE', #11975, 88.00000000000000000 ) ;
#1405 = ADVANCED_FACE ( 'NONE', ( #165 ), #3802, .F. ) ;
#1406 = PLANE ( 'NONE',  #3872 ) ;
#1407 = DIRECTION ( 'NONE',  ( 1.000000000000000000, 0.000000000000000000, 0.000000000000000000 ) ) ;
#1408 = ORIENTED_EDGE ( 'NONE', *, *, #19959, .F. ) ;
#1409 = CYLINDRICAL_SURFACE ( 'NONE', #2364, 45.00000000000000000 ) ;
#1410 = ORIENTED_EDGE ( 'NONE', *, *, #9707, .F. ) ;
#1411 = EDGE_CURVE ( 'NONE', #3473, #4200, #3064, .T. ) ;
#1412 = LINE ( 'NONE', #17762, #14791 ) ;
#1413 = DIRECTION ( 'NONE',  ( 0.000000000000000000, 0.000000000000000000, 1.000000000000000000 ) ) ;
#1414 = ORIENTED_EDGE ( 'NONE', *, *, #18533, .T. ) ;
#1415 = LINE ( 'NONE', #9458, #15187 ) ;
#1416 = ORIENTED_EDGE ( 'NONE', *, *, #7888, .F. ) ;
#1417 = ORIENTED_EDGE ( 'NONE', *, *, #2720, .F. ) ;
#1418 = CYLINDRICAL_SURFACE ( 'NONE', #16406, 92.50100000000000477 ) ;
#1419 = CIRCLE ( 'NONE', #699, 115.1000000000000227 ) ;
#1420 = ORIENTED_EDGE ( 'NONE', *, *, #15564, .F. ) ;
#1421 = CARTESIAN_POINT ( 'NONE',  ( 10.00000000000000000, 19.85071254963803611, -20.01672328094512565 ) ) ;
#1422 = DIRECTION ( 'NONE',  ( 1.000000000000000000, 0.000000000000000000, 0.000000000000000000 ) ) ;
#1423 = DIRECTION ( 'NONE',  ( 0.000000000000000000, -0.8660254037844432595, 0.4999999999999920064 ) ) ;
#1424 = DIRECTION ( 'NONE',  ( 0.000000000000000000, 0.000000000000000000, 1.000000000000000000 ) ) ;
#1425 = CARTESIAN_POINT ( 'NONE',  ( 10.00000000000000000, 0.000000000000000000, 0.000000000000000000 ) ) ;
#1426 = DIRECTION ( 'NONE',  ( -1.000000000000000000, 0.000000000000000000, 0.000000000000000000 ) ) ;
#1427 = CARTESIAN_POINT ( 'NONE',  ( 0.000000000000000000, -87.44637528609668209, 9.855528870798345054 ) ) ;
#1428 = EDGE_CURVE ( 'NONE', #18773, #7709, #15405, .T. ) ;
#1429 = CARTESIAN_POINT ( 'NONE',  ( 10.00000000000000000, 36.60317927562579854, 76.78148674856777234 ) ) ;
#1430 = DIRECTION ( 'NONE',  ( 0.000000000000000000, -0.9271838545667908660, 0.3746065934159032440 ) ) ;
#1431 = DIRECTION ( 'NONE',  ( 1.000000000000000000, 0.000000000000000000, 0.000000000000000000 ) ) ;
#1432 = PLANE ( 'NONE',  #13990 ) ;
#1433 = VERTEX_POINT ( 'NONE', #15288 ) ;
#1434 = ORIENTED_EDGE ( 'NONE', *, *, #5820, .F. ) ;
#1435 = VERTEX_POINT ( 'NONE', #10218 ) ;
#1436 = ORIENTED_EDGE ( 'NONE', *, *, #13673, .F. ) ;
#1437 = ORIENTED_EDGE ( 'NONE', *, *, #9467, .F. ) ;
#1438 = DIRECTION ( 'NONE',  ( 1.000000000000000000, 0.000000000000000000, 0.000000000000000000 ) ) ;
#1439 = VERTEX_POINT ( 'NONE', #11874 ) ;
#1440 = CYLINDRICAL_SURFACE ( 'NONE', #16326, 44.99999999999999289 ) ;
#1441 = AXIS2_PLACEMENT_3D ( 'NONE', #1677, #1785, #8419 ) ;
#1442 = DIRECTION ( 'NONE',  ( -1.000000000000000000, -0.000000000000000000, 0.000000000000000000 ) ) ;
#1443 = CYLINDRICAL_SURFACE ( 'NONE', #8906, 88.00000000000000000 ) ;
#1444 = DIRECTION ( 'NONE',  ( 0.000000000000000000, 0.7880107536067190166, 0.6156614753256620665 ) ) ;
#1445 = DIRECTION ( 'NONE',  ( -1.000000000000000000, 0.000000000000000000, 0.000000000000000000 ) ) ;
#1446 = DIRECTION ( 'NONE',  ( -1.000000000000000000, 0.000000000000000000, 0.000000000000000000 ) ) ;
#1447 = ORIENTED_EDGE ( 'NONE', *, *, #12333, .F. ) ;
#1448 = DIRECTION ( 'NONE',  ( -1.000000000000000000, -0.000000000000000000, -0.000000000000000000 ) ) ;
#1449 = VERTEX_POINT ( 'NONE', #8978 ) ;
#1450 = ORIENTED_EDGE ( 'NONE', *, *, #2028, .T. ) ;
#1451 = DIRECTION ( 'NONE',  ( 0.000000000000000000, 0.000000000000000000, -1.000000000000000000 ) ) ;
#1452 = ORIENTED_EDGE ( 'NONE', *, *, #9538, .T. ) ;
#1453 = CARTESIAN_POINT ( 'NONE',  ( 0.000000000000000000, 85.05652083079334602, 0.7600687895874258526 ) ) ;
#1454 = ORIENTED_EDGE ( 'NONE', *, *, #18800, .F. ) ;
#1455 = EDGE_LOOP ( 'NONE', ( #11743, #5949, #5509, #16369 ) ) ;
#1456 = DIRECTION ( 'NONE',  ( 0.000000000000000000, -0.7431448254773999063, 0.6691306063588517983 ) ) ;
#1457 = ORIENTED_EDGE ( 'NONE', *, *, #9041, .F. ) ;
#1458 = LINE ( 'NONE', #1569, #6882 ) ;
#1459 = CARTESIAN_POINT ( 'NONE',  ( 10.00000000000000000, 0.000000000000000000, 0.000000000000000000 ) ) ;
#1461 = AXIS2_PLACEMENT_3D ( 'NONE', #17185, #15619, #15402 ) ;
#1460 = DIRECTION ( 'NONE',  ( 0.000000000000000000, 0.000000000000000000, 1.000000000000000000 ) ) ;
#1462 = CARTESIAN_POINT ( 'NONE',  ( 10.00000000000000000, 83.89484365856945658, -26.56417150042864961 ) ) ;
#1463 = EDGE_CURVE ( 'NONE', #1099, #19677, #945, .T. ) ;
#1464 = DIRECTION ( 'NONE',  ( 1.000000000000000000, 0.000000000000000000, 0.000000000000000000 ) ) ;
#1465 = AXIS2_PLACEMENT_3D ( 'NONE', #14389, #17710, #12727 ) ;
#1466 = DIRECTION ( 'NONE',  ( 0.000000000000000000, 0.000000000000000000, 1.000000000000000000 ) ) ;
#1467 = CARTESIAN_POINT ( 'NONE',  ( 10.00000000000000000, 27.82509854686817263, -4.525913221810857756 ) ) ;
#1468 = CARTESIAN_POINT ( 'NONE',  ( 0.000000000000000000, -39.87723064937059547, -83.46401306393613595 ) ) ;
#1469 = ORIENTED_EDGE ( 'NONE', *, *, #19172, .F. ) ;
#1470 = EDGE_CURVE ( 'NONE', #11833, #2563, #5467, .T. ) ;
#1471 = DIRECTION ( 'NONE',  ( -1.000000000000000000, -0.000000000000000000, -0.000000000000000000 ) ) ;
#1472 = EDGE_CURVE ( 'NONE', #6262, #13819, #16119, .T. ) ;
#1473 = CYLINDRICAL_SURFACE ( 'NONE', #18362, 2.799999999999996714 ) ;
#1474 = ORIENTED_EDGE ( 'NONE', *, *, #427, .F. ) ;
#1475 = ORIENTED_EDGE ( 'NONE', *, *, #3523, .T. ) ;
#1476 = CARTESIAN_POINT ( 'NONE',  ( 10.00000000000000000, -36.39558101400191248, 80.12091913260368869 ) ) ;
#1477 = VERTEX_POINT ( 'NONE', #8668 ) ;
#1478 = ORIENTED_EDGE ( 'NONE', *, *, #2597, .T. ) ;
#1479 = CARTESIAN_POINT ( 'NONE',  ( 1.129531546211678616, 0.000000000000000000, 0.000000000000000000 ) ) ;
#1480 = ORIENTED_EDGE ( 'NONE', *, *, #4866, .T. ) ;
#1481 = EDGE_LOOP ( 'NONE', ( #15119, #8761, #15682, #11730 ) ) ;
#1482 = CARTESIAN_POINT ( 'NONE',  ( 1.399999999999999245, 0.000000000000000000, -7.400000000000020783 ) ) ;
#1483 = CARTESIAN_POINT ( 'NONE',  ( 5.000000000000002665, 73.32282170386848463, 48.65967342042805655 ) ) ;
#1484 = ORIENTED_EDGE ( 'NONE', *, *, #10253, .T. ) ;
#1485 = ADVANCED_FACE ( 'NONE', ( #20388 ), #10859, .T. ) ;
#1486 = AXIS2_PLACEMENT_3D ( 'NONE', #20493, #17289, #3477 ) ;
#1487 = DIRECTION ( 'NONE',  ( -1.000000000000000000, 0.000000000000000000, 0.000000000000000000 ) ) ;
#1488 = CARTESIAN_POINT ( 'NONE',  ( 5.000000000000002665, 6.797690662956386021, -87.73705831432209834 ) ) ;
#1489 = ADVANCED_FACE ( 'NONE', ( #11984 ), #18731, .F. ) ;
#1490 = CARTESIAN_POINT ( 'NONE',  ( -10.00000000000000000, 0.000000000000000000, 0.000000000000000000 ) ) ;
#1491 = EDGE_CURVE ( 'NONE', #2109, #20211, #15614, .T. ) ;
#1492 = CARTESIAN_POINT ( 'NONE',  ( 0.000000000000000000, 0.000000000000000000, 0.000000000000000000 ) ) ;
#1493 = CARTESIAN_POINT ( 'NONE',  ( 10.00000000000000000, 68.93609746931163329, 54.69748134696484954 ) ) ;
#1494 = CARTESIAN_POINT ( 'NONE',  ( 0.000000000000000000, 72.53479564998782791, 44.42851404693380601 ) ) ;
#1495 = UNCERTAINTY_MEASURE_WITH_UNIT (LENGTH_MEASURE( 1.000000000000000082E-05 ), #15175, 'distance_accuracy_value', 'NONE');
#1496 = EDGE_CURVE ( 'NONE', #10884, #20540, #3691, .T. ) ;
#1497 = ORIENTED_EDGE ( 'NONE', *, *, #8425, .T. ) ;
#1498 = FACE_OUTER_BOUND ( 'NONE', #4002, .T. ) ;
#1499 = CIRCLE ( 'NONE', #14541, 92.50100000000000477 ) ;
#1500 = CARTESIAN_POINT ( 'NONE',  ( 10.00000000000000000, 0.000000000000000000, 0.000000000000000000 ) ) ;
#1501 = ORIENTED_EDGE ( 'NONE', *, *, #4741, .F. ) ;
#1502 = DIRECTION ( 'NONE',  ( 0.000000000000000000, 0.000000000000000000, 1.000000000000000000 ) ) ;
#1503 = EDGE_CURVE ( 'NONE', #750, #2613, #7122, .T. ) ;
#1504 = ORIENTED_EDGE ( 'NONE', *, *, #4914, .T. ) ;
#1505 = DIRECTION ( 'NONE',  ( 1.000000000000000000, 0.000000000000000000, -0.000000000000000000 ) ) ;
#1506 = DIRECTION ( 'NONE',  ( -1.000000000000000000, 0.000000000000000000, 0.000000000000000000 ) ) ;
#1507 = ORIENTED_EDGE ( 'NONE', *, *, #15912, .F. ) ;
#1508 = EDGE_CURVE ( 'NONE', #9443, #9115, #488, .T. ) ;
#1509 = ORIENTED_EDGE ( 'NONE', *, *, #20060, .F. ) ;
#1510 = ORIENTED_EDGE ( 'NONE', *, *, #6218, .T. ) ;
#1511 = CARTESIAN_POINT ( 'NONE',  ( 0.000000000000000000, 46.93287725819779155, 70.94007663282461351 ) ) ;
#1512 = ORIENTED_EDGE ( 'NONE', *, *, #11078, .F. ) ;
#1513 = CARTESIAN_POINT ( 'NONE',  ( 150.0000507999999968, 0.000000000000000000, 0.000000000000000000 ) ) ;
#1514 = AXIS2_PLACEMENT_3D ( 'NONE', #17451, #10596, #3963 ) ;
#1515 = LINE ( 'NONE', #7821, #8632 ) ;
#1516 = DIRECTION ( 'NONE',  ( 0.000000000000000000, -0.9993908270190953180, -0.03489949670251103753 ) ) ;
#1517 = CARTESIAN_POINT ( 'NONE',  ( 10.00000000000000000, -8.134922360105496963, -84.67002113262489615 ) ) ;
#1518 = CARTESIAN_POINT ( 'NONE',  ( 10.00000000000000000, 9.992993448021589842, 26.36019881529889020 ) ) ;
#1519 = AXIS2_PLACEMENT_3D ( 'NONE', #7177, #17128, #1988 ) ;
#1520 = CIRCLE ( 'NONE', #12458, 11.99999999999999822 ) ;
#1521 = EDGE_CURVE ( 'NONE', #19720, #739, #10639, .T. ) ;
#1522 = LINE ( 'NONE', #15000, #2381 ) ;
#1523 = DIRECTION ( 'NONE',  ( -1.000000000000000000, -0.000000000000000000, 0.000000000000000000 ) ) ;
#1524 = AXIS2_PLACEMENT_3D ( 'NONE', #10527, #14164, #20907 ) ;
#1525 = DIRECTION ( 'NONE',  ( 0.000000000000000000, 0.000000000000000000, 1.000000000000000000 ) ) ;
#1526 = CARTESIAN_POINT ( 'NONE',  ( 10.00000000000000000, 75.87763420127893710, -44.57111876559645225 ) ) ;
#1527 = CARTESIAN_POINT ( 'NONE',  ( 0.000000000000000000, 37.96946988134172329, 76.11510229470873412 ) ) ;
#1528 = EDGE_CURVE ( 'NONE', #18417, #16782, #7448, .T. ) ;
#1529 = VERTEX_POINT ( 'NONE', #802 ) ;
#1530 = CIRCLE ( 'NONE', #16337, 5.000000000000000888 ) ;
#1531 = CYLINDRICAL_SURFACE ( 'NONE', #20778, 88.00000000000000000 ) ;
#1532 = EDGE_LOOP ( 'NONE', ( #8337, #17524, #20603, #12767 ) ) ;
#1533 = EDGE_CURVE ( 'NONE', #15558, #11042, #15456, .T. ) ;
#1534 = ORIENTED_EDGE ( 'NONE', *, *, #6971, .T. ) ;
#1535 = CIRCLE ( 'NONE', #19877, 44.99999999999998579 ) ;
#1536 = VERTEX_POINT ( 'NONE', #17620 ) ;
#1537 = EDGE_CURVE ( 'NONE', #20116, #18424, #13695, .T. ) ;
#1538 = AXIS2_PLACEMENT_3D ( 'NONE', #3716, #11687, #17203 ) ;
#1539 = EDGE_CURVE ( 'NONE', #21817, #5871, #12841, .T. ) ;
#1540 = EDGE_LOOP ( 'NONE', ( #6165, #4258 ) ) ;
#1541 = LINE ( 'NONE', #13250, #4532 ) ;
#1542 = AXIS2_PLACEMENT_3D ( 'NONE', #18159, #16603, #21791 ) ;
#1543 = VERTEX_POINT ( 'NONE', #16167 ) ;
#1544 = CARTESIAN_POINT ( 'NONE',  ( 0.000000000000000000, -41.21966518006011881, 82.80926399530274296 ) ) ;
#1545 = CARTESIAN_POINT ( 'NONE',  ( -10.00000000000000000, 0.000000000000000000, 0.000000000000000000 ) ) ;
#1546 = AXIS2_PLACEMENT_3D ( 'NONE', #7056, #20313, #8701 ) ;
#1547 = DIRECTION ( 'NONE',  ( 0.000000000000000000, 0.000000000000000000, 1.000000000000000000 ) ) ;
#1548 = CARTESIAN_POINT ( 'NONE',  ( 10.00000000000000000, -18.94217447942500598, -85.93715160505971085 ) ) ;
#1549 = DIRECTION ( 'NONE',  ( -1.000000000000000000, 0.000000000000000000, 0.000000000000000000 ) ) ;
#1550 = DIRECTION ( 'NONE',  ( -1.000000000000000000, 0.000000000000000000, -0.000000000000000000 ) ) ;
#1551 = FACE_OUTER_BOUND ( 'NONE', #20491, .T. ) ;
#1552 = AXIS2_PLACEMENT_3D ( 'NONE', #2014, #5226, #1800 ) ;
#1553 = EDGE_LOOP ( 'NONE', ( #10951, #17472, #17504, #2375 ) ) ;
#1554 = PRODUCT_DEFINITION_SHAPE ( 'NONE', 'NONE',  #21863 ) ;
#1555 = CIRCLE ( 'NONE', #8604, 92.50099999999999056 ) ;
#1556 = CARTESIAN_POINT ( 'NONE',  ( 1.500000000000001332, 0.000000000000000000, 0.000000000000000000 ) ) ;
#1557 = ORIENTED_EDGE ( 'NONE', *, *, #1864, .T. ) ;
#1558 = VERTEX_POINT ( 'NONE', #916 ) ;
#1559 = CARTESIAN_POINT ( 'NONE',  ( 10.00000000000000000, -32.56745702629792305, 78.57830605990643846 ) ) ;
#1560 = AXIS2_PLACEMENT_3D ( 'NONE', #18307, #3156, #9890 ) ;
#1561 = ORIENTED_EDGE ( 'NONE', *, *, #8114, .T. ) ;
#1562 = DIRECTION ( 'NONE',  ( -1.000000000000000000, -0.000000000000000000, -0.000000000000000000 ) ) ;
#1563 = ORIENTED_EDGE ( 'NONE', *, *, #13508, .T. ) ;
#1564 = ORIENTED_EDGE ( 'NONE', *, *, #5961, .F. ) ;
#1565 = CONTEXT_DEPENDENT_SHAPE_REPRESENTATION ( #9810, #6700 ) ;
#1566 = AXIS2_PLACEMENT_3D ( 'NONE', #9885, #1487, #21390 ) ;
#1567 = CARTESIAN_POINT ( 'NONE',  ( -90.00000000000000000, 0.000000000000000000, 0.000000000000000000 ) ) ;
#1568 = ORIENTED_EDGE ( 'NONE', *, *, #6891, .F. ) ;
#1569 = CARTESIAN_POINT ( 'NONE',  ( 10.00000000000000000, 10.41137886060107576, 91.91321010181850681 ) ) ;
#1570 = CIRCLE ( 'NONE', #12149, 6.887500000000022382 ) ;
#1571 = CARTESIAN_POINT ( 'NONE',  ( 10.00000000000000000, 0.000000000000000000, 0.000000000000000000 ) ) ;
#1572 = DIRECTION ( 'NONE',  ( -1.000000000000000000, -0.000000000000000000, 0.000000000000000000 ) ) ;
#1573 = DIRECTION ( 'NONE',  ( -1.000000000000000000, 0.000000000000000000, 0.000000000000000000 ) ) ;
#1574 = SURFACE_STYLE_USAGE ( .BOTH. , #14727 ) ;
#1575 = DIRECTION ( 'NONE',  ( -0.000000000000000000, -0.000000000000000000, 1.000000000000000000 ) ) ;
#1576 = CARTESIAN_POINT ( 'NONE',  ( 10.00000000000000000, -12.90282758292962662, -25.06465718894790484 ) ) ;
#1577 = DIRECTION ( 'NONE',  ( 1.000000000000000000, 0.000000000000000000, 0.000000000000000000 ) ) ;
#1578 = AXIS2_PLACEMENT_3D ( 'NONE', #19110, #15572, #5636 ) ;
#1579 = AXIS2_PLACEMENT_3D ( 'NONE', #10140, #8382, #3081 ) ;
#1580 = ORIENTED_EDGE ( 'NONE', *, *, #18346, .T. ) ;
#1581 = CIRCLE ( 'NONE', #11820, 44.99999999999999289 ) ;
#1582 = CIRCLE ( 'NONE', #2981, 92.50100000000000477 ) ;
#1583 = TOROIDAL_SURFACE ( 'NONE', #20640, 114.9007999999999896, 0.2042000000000016025 ) ;
#1584 = DIRECTION ( 'NONE',  ( 1.000000000000000000, 0.000000000000000000, -0.000000000000000000 ) ) ;
#1585 = DIRECTION ( 'NONE',  ( 1.000000000000000000, 0.000000000000000000, 0.000000000000000000 ) ) ;
#1586 = VERTEX_POINT ( 'NONE', #12625 ) ;
#1587 = EDGE_CURVE ( 'NONE', #1246, #1789, #17719, .T. ) ;
#1588 = CARTESIAN_POINT ( 'NONE',  ( 10.00000000000000000, -9.366510754379408610, 25.85466064925422458 ) ) ;
#1589 = ORIENTED_EDGE ( 'NONE', *, *, #12560, .F. ) ;
#1590 = ORIENTED_EDGE ( 'NONE', *, *, #6143, .F. ) ;
#1591 = FACE_OUTER_BOUND ( 'NONE', #14853, .T. ) ;
#1592 = VERTEX_POINT ( 'NONE', #12737 ) ;
#1593 = AXIS2_PLACEMENT_3D ( 'NONE', #19189, #7483, #17757 ) ;
#1594 = VERTEX_POINT ( 'NONE', #1035 ) ;
#1595 = FACE_OUTER_BOUND ( 'NONE', #6372, .T. ) ;
#1596 = DIRECTION ( 'NONE',  ( -1.000000000000000000, 0.000000000000000000, -0.000000000000000000 ) ) ;
#1597 = AXIS2_PLACEMENT_3D ( 'NONE', #2134, #13512, #12295 ) ;
#1598 = ADVANCED_FACE ( 'NONE', ( #11080 ), #19377, .F. ) ;
#1599 = ORIENTED_EDGE ( 'NONE', *, *, #19434, .T. ) ;
#1600 = AXIS2_PLACEMENT_3D ( 'NONE', #21822, #1718, #11556 ) ;
#1601 = AXIS2_PLACEMENT_3D ( 'NONE', #15817, #20790, #462 ) ;
#1602 = CYLINDRICAL_SURFACE ( 'NONE', #13215, 88.00000000000000000 ) ;
#1603 = DIRECTION ( 'NONE',  ( -1.000000000000000000, -0.000000000000000000, -0.000000000000000000 ) ) ;
#1604 = FACE_OUTER_BOUND ( 'NONE', #18499, .T. ) ;
#1605 = LINE ( 'NONE', #15075, #10024 ) ;
#1606 = DIRECTION ( 'NONE',  ( 0.000000000000000000, 0.000000000000000000, 1.000000000000000000 ) ) ;
#1607 = CARTESIAN_POINT ( 'NONE',  ( 0.000000000000000000, -51.18896083639217665, -71.57995730992236361 ) ) ;
#1608 = CIRCLE ( 'NONE', #15721, 92.50100000000000477 ) ;
#1609 = VERTEX_POINT ( 'NONE', #14398 ) ;
#1610 = CYLINDRICAL_SURFACE ( 'NONE', #15878, 44.99999999999998579 ) ;
#1611 = DIRECTION ( 'NONE',  ( -1.000000000000000000, 0.000000000000000000, 0.000000000000000000 ) ) ;
#1612 = ORIENTED_EDGE ( 'NONE', *, *, #473, .T. ) ;
#1613 = CIRCLE ( 'NONE', #5156, 32.00000000000000000 ) ;
#1614 = AXIS2_PLACEMENT_3D ( 'NONE', #13529, #489, #20279 ) ;
#1615 = CARTESIAN_POINT ( 'NONE',  ( 10.00000000000000000, -25.56104204395359503, 81.12843256239655432 ) ) ;
#1616 = AXIS2_PLACEMENT_3D ( 'NONE', #16141, #2777, #9387 ) ;
#1617 = EDGE_LOOP ( 'NONE', ( #7199, #15983, #11344, #1051 ) ) ;
#1618 = EDGE_CURVE ( 'NONE', #3657, #11363, #3460, .T. ) ;
#1619 = ADVANCED_FACE ( 'NONE', ( #2570 ), #2356, .T. ) ;
#1620 = EDGE_CURVE ( 'NONE', #8870, #18369, #7699, .T. ) ;
#1621 = DIRECTION ( 'NONE',  ( 1.000000000000000000, 0.000000000000000000, 0.000000000000000000 ) ) ;
#1622 = ORIENTED_EDGE ( 'NONE', *, *, #21444, .F. ) ;
#1623 = CARTESIAN_POINT ( 'NONE',  ( 10.00000000000000000, 11.59241532900628258, 87.23311244498744088 ) ) ;
#1624 = EDGE_CURVE ( 'NONE', #20752, #12067, #9096, .T. ) ;
#1625 = VERTEX_POINT ( 'NONE', #17943 ) ;
#1626 = ORIENTED_EDGE ( 'NONE', *, *, #6269, .F. ) ;
#1627 = ORIENTED_EDGE ( 'NONE', *, *, #17106, .T. ) ;
#1628 = CARTESIAN_POINT ( 'NONE',  ( 10.00000000000000000, -65.64563793391867819, 54.09103124042793098 ) ) ;
#1629 = CIRCLE ( 'NONE', #13972, 88.00000000000000000 ) ;
#1630 = EDGE_LOOP ( 'NONE', ( #3742, #9026, #11606, #14649 ) ) ;
#1631 = APPLICATION_CONTEXT ( 'automotive_design' ) ;
#1632 = DIRECTION ( 'NONE',  ( -1.000000000000000000, 0.000000000000000000, -0.000000000000000000 ) ) ;
#1633 = CARTESIAN_POINT ( 'NONE',  ( -8.900000000000019895, 0.000000000000000000, 0.000000000000000000 ) ) ;
#1634 = CARTESIAN_POINT ( 'NONE',  ( 0.000000000000000000, 0.000000000000000000, 0.000000000000000000 ) ) ;
#1635 = VECTOR ( 'NONE', #8939, 1000.000000000000000 ) ;
#1636 = DIRECTION ( 'NONE',  ( 0.000000000000000000, 0.000000000000000000, 1.000000000000000000 ) ) ;
#1637 = AXIS2_PLACEMENT_3D ( 'NONE', #4015, #2357, #4458 ) ;
#1638 = EDGE_CURVE ( 'NONE', #11791, #13591, #21809, .T. ) ;
#1639 = CIRCLE ( 'NONE', #4406, 27.49900000000000233 ) ;
#1640 = CARTESIAN_POINT ( 'NONE',  ( 10.00000000000000000, 70.37753541436022431, -60.02863908169562279 ) ) ;
#1641 = CARTESIAN_POINT ( 'NONE',  ( 10.00000000000000000, 87.58454185039451545, -8.540961822680756654 ) ) ;
#1642 = EDGE_CURVE ( 'NONE', #11604, #21750, #15801, .T. ) ;
#1643 = DIRECTION ( 'NONE',  ( 0.000000000000000000, 0.000000000000000000, 1.000000000000000000 ) ) ;
#1644 = DIRECTION ( 'NONE',  ( -1.000000000000000000, -0.000000000000000000, 0.000000000000000000 ) ) ;
#1645 = DIRECTION ( 'NONE',  ( -1.000000000000000000, -0.000000000000000000, 0.000000000000000000 ) ) ;
#1646 = ORIENTED_EDGE ( 'NONE', *, *, #20959, .F. ) ;
#1647 = FILL_AREA_STYLE ('',( #16781 ) ) ;
#1648 = AXIS2_PLACEMENT_3D ( 'NONE', #10143, #11361, #13127 ) ;
#1649 = EDGE_CURVE ( 'NONE', #8568, #7280, #14510, .T. ) ;
#1650 = EDGE_LOOP ( 'NONE', ( #20054, #7165, #4558, #9351 ) ) ;
#1651 = PLANE ( 'NONE',  #14411 ) ;
#1652 = AXIS2_PLACEMENT_3D ( 'NONE', #682, #5658, #1008 ) ;
#1653 = ORIENTED_EDGE ( 'NONE', *, *, #4765, .T. ) ;
#1654 = EDGE_CURVE ( 'NONE', #2973, #3104, #5936, .T. ) ;
#1655 = VERTEX_POINT ( 'NONE', #9524 ) ;
#1656 = VERTEX_POINT ( 'NONE', #21151 ) ;
#1657 = CARTESIAN_POINT ( 'NONE',  ( -1.500346250137462226E-14, 60.00000000000001421, 0.000000000000000000 ) ) ;
#1658 = EDGE_LOOP ( 'NONE', ( #13864, #6422, #15295, #16148 ) ) ;
#1659 = DIRECTION ( 'NONE',  ( -1.000000000000000000, -0.000000000000000000, 0.000000000000000000 ) ) ;
#1660 = DIRECTION ( 'NONE',  ( -1.000000000000000000, 0.000000000000000000, 0.000000000000000000 ) ) ;
#1661 = EDGE_CURVE ( 'NONE', #14806, #6246, #6021, .T. ) ;
#1662 = VECTOR ( 'NONE', #11381, 1000.000000000000000 ) ;
#1663 = DIRECTION ( 'NONE',  ( -1.000000000000000000, -0.000000000000000000, 0.000000000000000000 ) ) ;
#1664 = CIRCLE ( 'NONE', #11180, 44.99999999999999289 ) ;
#1665 = FACE_OUTER_BOUND ( 'NONE', #12587, .T. ) ;
#1666 = EDGE_CURVE ( 'NONE', #1099, #19664, #12402, .T. ) ;
#1667 = CIRCLE ( 'NONE', #14007, 104.9000000000000341 ) ;
#1668 = CARTESIAN_POINT ( 'NONE',  ( 10.00000000000000000, -31.88200538760795766, 2.745493118646876951 ) ) ;
#1669 = CYLINDRICAL_SURFACE ( 'NONE', #14435, 92.50100000000000477 ) ;
#1670 = ADVANCED_FACE ( 'NONE', ( #10748 ), #16382, .F. ) ;
#1671 = ORIENTED_EDGE ( 'NONE', *, *, #2549, .T. ) ;
#1672 = ADVANCED_FACE ( 'NONE', ( #6681 ), #11527, .F. ) ;
#1673 = CARTESIAN_POINT ( 'NONE',  ( 10.00000000000000000, 0.000000000000000000, 0.000000000000000000 ) ) ;
#1674 = ORIENTED_EDGE ( 'NONE', *, *, #1906, .F. ) ;
#1675 = ORIENTED_EDGE ( 'NONE', *, *, #15133, .T. ) ;
#1676 = AXIS2_PLACEMENT_3D ( 'NONE', #9689, #2860, #6415 ) ;
#1677 = CARTESIAN_POINT ( 'NONE',  ( 10.00000000000000000, -84.12297548659712731, -12.59025161327086906 ) ) ;
#1678 = EDGE_CURVE ( 'NONE', #628, #13720, #3106, .T. ) ;
#1679 = ORIENTED_EDGE ( 'NONE', *, *, #15846, .F. ) ;
#1680 = CARTESIAN_POINT ( 'NONE',  ( 0.000000000000000000, 10.41137886060228901, -91.91321010181836471 ) ) ;
#1681 = ORIENTED_EDGE ( 'NONE', *, *, #10837, .T. ) ;
#1682 = ORIENTED_EDGE ( 'NONE', *, *, #15928, .T. ) ;
#1683 = AXIS2_PLACEMENT_3D ( 'NONE', #6953, #18660, #20525 ) ;
#1684 = SHAPE_DEFINITION_REPRESENTATION ( #10206, #6721 ) ;
#1685 = DIRECTION ( 'NONE',  ( 0.000000000000000000, 0.000000000000000000, 1.000000000000000000 ) ) ;
#1686 = VERTEX_POINT ( 'NONE', #13283 ) ;
#1687 = DIRECTION ( 'NONE',  ( 0.000000000000000000, 0.000000000000000000, -1.000000000000000000 ) ) ;
#1688 = PLANE ( 'NONE',  #20653 ) ;
#1689 = DIRECTION ( 'NONE',  ( 0.000000000000000000, 0.6946583704589984753, -0.7193398003386500816 ) ) ;
#1690 = DIRECTION ( 'NONE',  ( 1.000000000000000000, -0.000000000000000000, 0.000000000000000000 ) ) ;
#1691 = DIRECTION ( 'NONE',  ( 0.000000000000000000, 0.000000000000000000, 1.000000000000000000 ) ) ;
#1692 = DIRECTION ( 'NONE',  ( 0.000000000000000000, 0.000000000000000000, 1.000000000000000000 ) ) ;
#1693 = DIRECTION ( 'NONE',  ( -1.000000000000000000, 0.000000000000000000, 0.000000000000000000 ) ) ;
#1694 = AXIS2_PLACEMENT_3D ( 'NONE', #14424, #17642, #2707 ) ;
#1695 = CIRCLE ( 'NONE', #2057, 88.00000000000000000 ) ;
#1696 = AXIS2_PLACEMENT_3D ( 'NONE', #20737, #12431, #3607 ) ;
#1697 = ORIENTED_EDGE ( 'NONE', *, *, #15237, .T. ) ;
#1698 = VECTOR ( 'NONE', #8210, 1000.000000000000000 ) ;
#1699 = EDGE_CURVE ( 'NONE', #10259, #19663, #7996, .T. ) ;
#1700 = LINE ( 'NONE', #8444, #5939 ) ;
#1701 = DIRECTION ( 'NONE',  ( 0.000000000000000000, 0.000000000000000000, 1.000000000000000000 ) ) ;
#1702 = ORIENTED_EDGE ( 'NONE', *, *, #7980, .T. ) ;
#1703 = CARTESIAN_POINT ( 'NONE',  ( 0.000000000000000000, 9.646732466566502850, -84.51112348751837544 ) ) ;
#1704 = ORIENTED_EDGE ( 'NONE', *, *, #7014, .F. ) ;
#1705 = SURFACE_SIDE_STYLE ('',( #16621 ) ) ;
#1706 = CIRCLE ( 'NONE', #7010, 44.99999999999999289 ) ;
#1707 = ORIENTED_EDGE ( 'NONE', *, *, #18953, .T. ) ;
#1708 = DIRECTION ( 'NONE',  ( 0.000000000000000000, 0.3420201433256693235, -0.9396926207859080948 ) ) ;
#1709 = ORIENTED_EDGE ( 'NONE', *, *, #6273, .T. ) ;
#1710 = VECTOR ( 'NONE', #18038, 1000.000000000000000 ) ;
#1711 = ORIENTED_EDGE ( 'NONE', *, *, #1870, .T. ) ;
#1712 = DIRECTION ( 'NONE',  ( 1.000000000000000000, 0.000000000000000000, 0.000000000000000000 ) ) ;
#1713 = CARTESIAN_POINT ( 'NONE',  ( 10.00000000000000000, -23.37352460145267941, -21.85585385440903394 ) ) ;
#1714 = AXIS2_PLACEMENT_3D ( 'NONE', #19789, #14919, #1227 ) ;
#1715 = ORIENTED_EDGE ( 'NONE', *, *, #11220, .T. ) ;
#1716 = DIRECTION ( 'NONE',  ( -1.000000000000000000, 0.000000000000000000, -0.000000000000000000 ) ) ;
#1717 = DIRECTION ( 'NONE',  ( -0.000000000000000000, -0.000000000000000000, -1.000000000000000000 ) ) ;
#1718 = DIRECTION ( 'NONE',  ( 0.000000000000000000, 1.000000000000000000, -1.224646799147353207E-16 ) ) ;
#1719 = DIRECTION ( 'NONE',  ( 0.000000000000000000, 4.085273785925381338E-14, -1.000000000000000000 ) ) ;
#1720 = CARTESIAN_POINT ( 'NONE',  ( 0.000000000000000000, 1.959304526718168571, -27.42911093658673138 ) ) ;
#1721 = DIRECTION ( 'NONE',  ( 0.000000000000000000, 0.8660254037844399289, -0.4999999999999979461 ) ) ;
#1722 = EDGE_CURVE ( 'NONE', #16061, #7775, #7193, .T. ) ;
#1723 = ORIENTED_EDGE ( 'NONE', *, *, #3809, .T. ) ;
#1724 = DIRECTION ( 'NONE',  ( -1.000000000000000000, 0.000000000000000000, -0.000000000000000000 ) ) ;
#1725 = CIRCLE ( 'NONE', #9466, 92.50100000000000477 ) ;
#1726 = CARTESIAN_POINT ( 'NONE',  ( 0.000000000000000000, 0.000000000000000000, 0.000000000000000000 ) ) ;
#1727 = ORIENTED_EDGE ( 'NONE', *, *, #19063, .T. ) ;
#1728 = CARTESIAN_POINT ( 'NONE',  ( -10.00000000000000000, 0.000000000000000000, 0.000000000000000000 ) ) ;
#1729 = EDGE_LOOP ( 'NONE', ( #5221, #16291, #20410, #6226 ) ) ;
#1730 = DIRECTION ( 'NONE',  ( 1.000000000000000000, 0.000000000000000000, 0.000000000000000000 ) ) ;
#1731 = FACE_OUTER_BOUND ( 'NONE', #3040, .T. ) ;
#1732 = ORIENTED_EDGE ( 'NONE', *, *, #3834, .F. ) ;
#1733 = FACE_OUTER_BOUND ( 'NONE', #6081, .T. ) ;
#1734 = ORIENTED_EDGE ( 'NONE', *, *, #16924, .F. ) ;
#1735 = ORIENTED_EDGE ( 'NONE', *, *, #9, .T. ) ;
#1736 = ORIENTED_EDGE ( 'NONE', *, *, #12188, .T. ) ;
#1737 = CARTESIAN_POINT ( 'NONE',  ( 0.000000000000000000, -7.240962358591358061, -31.16999300804322104 ) ) ;
#1738 = EDGE_LOOP ( 'NONE', ( #4235, #16570, #14554, #8920 ) ) ;
#1739 = FACE_OUTER_BOUND ( 'NONE', #2617, .T. ) ;
#1740 = CARTESIAN_POINT ( 'NONE',  ( 0.000000000000000000, 0.000000000000000000, 0.000000000000000000 ) ) ;
#1741 = CARTESIAN_POINT ( 'NONE',  ( 10.00000000000000000, -52.34334029047821701, -76.26670130689538496 ) ) ;
#1742 = VECTOR ( 'NONE', #20832, 1000.000000000000000 ) ;
#1743 = CARTESIAN_POINT ( 'NONE',  ( 0.000000000000000000, 0.000000000000000000, 0.000000000000000000 ) ) ;
#1744 = AXIS2_PLACEMENT_3D ( 'NONE', #2260, #19067, #13979 ) ;
#1746 = AXIS2_PLACEMENT_3D ( 'NONE', #8270, #2756, #9478 ) ;
#1745 = PRODUCT ( 'internal spur gear_iso_ISO - Internal spur gear 2M 90T 20PA 10FW ---S90S200OD 1.0AF', 'internal spur gear_iso_ISO - Internal spur gear 2M 90T 20PA 10FW ---S90S200OD 1.0AF', '', ( #4992 ) ) ;
#1747 = DIRECTION ( 'NONE',  ( -1.000000000000000000, -0.000000000000000000, 0.000000000000000000 ) ) ;
#1748 = EDGE_CURVE ( 'NONE', #1308, #12422, #19169, .T. ) ;
#1749 = DIRECTION ( 'NONE',  ( 0.000000000000000000, -0.8290375725550350738, -0.5591929034707565638 ) ) ;
#1750 = CARTESIAN_POINT ( 'NONE',  ( 0.000000000000000000, -87.44637528609653998, -9.855528870799524555 ) ) ;
#1751 = DIRECTION ( 'NONE',  ( -1.000000000000000000, -0.000000000000000000, -0.000000000000000000 ) ) ;
#1752 = CARTESIAN_POINT ( 'NONE',  ( 0.000000000000000000, -84.33453774737651543, -11.08490790852216534 ) ) ;
#1753 = FACE_OUTER_BOUND ( 'NONE', #3852, .T. ) ;
#1754 = CIRCLE ( 'NONE', #2813, 92.50100000000000477 ) ;
#1755 = ORIENTED_EDGE ( 'NONE', *, *, #13137, .F. ) ;
#1756 = DIRECTION ( 'NONE',  ( 0.000000000000000000, 0.000000000000000000, 1.000000000000000000 ) ) ;
#1757 = ORIENTED_EDGE ( 'NONE', *, *, #2328, .F. ) ;
#1758 = AXIS2_PLACEMENT_3D ( 'NONE', #17735, #14521, #21488 ) ;
#1759 = DIRECTION ( 'NONE',  ( -1.000000000000000000, -0.000000000000000000, 0.000000000000000000 ) ) ;
#1760 = VECTOR ( 'NONE', #17870, 1000.000000000000000 ) ;
#1761 = EDGE_LOOP ( 'NONE', ( #16780, #17714, #19772, #15246 ) ) ;
#1762 = ADVANCED_FACE ( 'NONE', ( #11734 ), #12122, .T. ) ;
#1763 = ORIENTED_EDGE ( 'NONE', *, *, #2386, .F. ) ;
#1764 = ORIENTED_EDGE ( 'NONE', *, *, #10681, .T. ) ;
#1765 = DIRECTION ( 'NONE',  ( 1.000000000000000000, 0.000000000000000000, 0.000000000000000000 ) ) ;
#1766 = VERTEX_POINT ( 'NONE', #8106 ) ;
#1767 = DIRECTION ( 'NONE',  ( 1.000000000000000000, 0.000000000000000000, 0.000000000000000000 ) ) ;
#1768 = CARTESIAN_POINT ( 'NONE',  ( 10.00000000000000000, 64.95266917914317162, 59.37298010462993858 ) ) ;
#1769 = EDGE_CURVE ( 'NONE', #6526, #5588, #20939, .T. ) ;
#1770 = DIRECTION ( 'NONE',  ( 0.000000000000000000, 0.9510565162951544194, -0.3090169943749448422 ) ) ;
#1771 = EDGE_CURVE ( 'NONE', #13577, #12634, #19883, .T. ) ;
#1772 = CARTESIAN_POINT ( 'NONE',  ( -90.00000000000000000, 0.000000000000000000, 0.000000000000000000 ) ) ;
#1773 = CARTESIAN_POINT ( 'NONE',  ( 10.00000000000000000, -21.69483248597433089, 16.89761061231773454 ) ) ;
#1774 = EDGE_CURVE ( 'NONE', #3544, #13981, #3998, .T. ) ;
#1775 = CIRCLE ( 'NONE', #20824, 44.99999999999999289 ) ;
#1776 = DIRECTION ( 'NONE',  ( -1.000000000000000000, 0.000000000000000000, -0.000000000000000000 ) ) ;
#1777 = CARTESIAN_POINT ( 'NONE',  ( 0.000000000000000000, 67.05625154133453236, 63.71729851637834940 ) ) ;
#1778 = ADVANCED_FACE ( 'NONE', ( #6239, #21681 ), #14615, .F. ) ;
#1779 = ORIENTED_EDGE ( 'NONE', *, *, #21178, .T. ) ;
#1780 = DIRECTION ( 'NONE',  ( 0.000000000000000000, 0.000000000000000000, 1.000000000000000000 ) ) ;
#1781 = EDGE_CURVE ( 'NONE', #11509, #16102, #15996, .T. ) ;
#1782 = ORIENTED_EDGE ( 'NONE', *, *, #14864, .T. ) ;
#1783 = ORIENTED_EDGE ( 'NONE', *, *, #19778, .F. ) ;
#1784 = EDGE_CURVE ( 'NONE', #9397, #10412, #6493, .T. ) ;
#1785 = DIRECTION ( 'NONE',  ( 1.000000000000000000, 0.000000000000000000, 0.000000000000000000 ) ) ;
#1786 = ORIENTED_EDGE ( 'NONE', *, *, #14688, .F. ) ;
#1787 = AXIS2_PLACEMENT_3D ( 'NONE', #19020, #15689, #3549 ) ;
#1788 = DIRECTION ( 'NONE',  ( 0.000000000000000000, 0.000000000000000000, 1.000000000000000000 ) ) ;
#1789 = VERTEX_POINT ( 'NONE', #14834 ) ;
#1790 = ORIENTED_EDGE ( 'NONE', *, *, #19319, .T. ) ;
#1791 = PRODUCT_CONTEXT ( 'NONE', #13199, 'mechanical' ) ;
#1792 = EDGE_CURVE ( 'NONE', #6729, #12424, #19809, .T. ) ;
#1793 = CARTESIAN_POINT ( 'NONE',  ( 0.000000000000000000, 78.80192417387979731, -39.16958956249220591 ) ) ;
#1794 = VERTEX_POINT ( 'NONE', #4670 ) ;
#1795 = CARTESIAN_POINT ( 'NONE',  ( 0.000000000000000000, 0.6609040254623582689, -87.99751818016873983 ) ) ;
#1796 = EDGE_CURVE ( 'NONE', #2646, #8089, #18835, .T. ) ;
#1797 = DIRECTION ( 'NONE',  ( -1.000000000000000000, -0.000000000000000000, -0.000000000000000000 ) ) ;
#1798 = CARTESIAN_POINT ( 'NONE',  ( 10.00000000000000000, -24.73395913766471921, 12.01774797440568854 ) ) ;
#1799 = CARTESIAN_POINT ( 'NONE',  ( 10.00000000000000000, 3.974475837764916530, 92.41557521768191918 ) ) ;
#1800 = DIRECTION ( 'NONE',  ( 0.000000000000000000, 0.2079116908177532363, 0.9781476007338069101 ) ) ;
#1801 = DIRECTION ( 'NONE',  ( -0.000000000000000000, -0.000000000000000000, -1.000000000000000000 ) ) ;
#1802 = DIRECTION ( 'NONE',  ( -1.000000000000000000, 0.000000000000000000, -0.000000000000000000 ) ) ;
#1803 = ADVANCED_FACE ( 'NONE', ( #15053 ), #16496, .F. ) ;
#1804 = ORIENTED_EDGE ( 'NONE', *, *, #8132, .F. ) ;
#1805 = CARTESIAN_POINT ( 'NONE',  ( 10.00000000000000000, -1.592605004252595213, -28.14575649959895998 ) ) ;
#1806 = FACE_OUTER_BOUND ( 'NONE', #10129, .T. ) ;
#1807 = VERTEX_POINT ( 'NONE', #1462 ) ;
#1808 = DIRECTION ( 'NONE',  ( 0.000000000000000000, 0.8660254037844362651, 0.5000000000000041078 ) ) ;
#1809 = ADVANCED_FACE ( 'NONE', ( #4896 ), #12463, .T. ) ;
#1810 = ORIENTED_EDGE ( 'NONE', *, *, #13767, .T. ) ;
#1811 = SURFACE_STYLE_USAGE ( .BOTH. , #15387 ) ;
#1812 = ORIENTED_EDGE ( 'NONE', *, *, #1539, .T. ) ;
#1813 = CARTESIAN_POINT ( 'NONE',  ( 0.000000000000000000, 0.000000000000000000, 0.000000000000000000 ) ) ;
#1814 = ORIENTED_EDGE ( 'NONE', *, *, #10137, .T. ) ;
#1815 = ORIENTED_EDGE ( 'NONE', *, *, #6236, .F. ) ;
#1816 =( GEOMETRIC_REPRESENTATION_CONTEXT ( 3 ) GLOBAL_UNCERTAINTY_ASSIGNED_CONTEXT ( ( #1495 ) ) GLOBAL_UNIT_ASSIGNED_CONTEXT ( ( #15175, #13183, #5240 ) ) REPRESENTATION_CONTEXT ( 'NONE', 'WORKASPACE' ) );
#1817 = ADVANCED_FACE ( 'NONE', ( #13609 ), #20249, .F. ) ;
#1818 = DIRECTION ( 'NONE',  ( 0.000000000000000000, 0.000000000000000000, 1.000000000000000000 ) ) ;
#1819 = LINE ( 'NONE', #16843, #13837 ) ;
#1820 = ORIENTED_EDGE ( 'NONE', *, *, #21401, .F. ) ;
#1821 = ADVANCED_FACE ( 'NONE', ( #7104 ), #3562, .F. ) ;
#1822 = CARTESIAN_POINT ( 'NONE',  ( 10.00000000000000000, 0.000000000000000000, 0.000000000000000000 ) ) ;
#1823 = DIRECTION ( 'NONE',  ( -1.000000000000000000, 0.000000000000000000, 0.000000000000000000 ) ) ;
#1824 = DIRECTION ( 'NONE',  ( -1.000000000000000000, 0.000000000000000000, 0.000000000000000000 ) ) ;
#1825 = DIRECTION ( 'NONE',  ( -1.000000000000000000, -0.000000000000000000, 0.000000000000000000 ) ) ;
#1826 = DIRECTION ( 'NONE',  ( 0.000000000000000000, 0.3420201433256693235, -0.9396926207859080948 ) ) ;
#1827 = ORIENTED_EDGE ( 'NONE', *, *, #6393, .F. ) ;
#1828 = CARTESIAN_POINT ( 'NONE',  ( 10.00000000000000000, 27.00677879429135331, -80.65868421664406185 ) ) ;
#1829 = DIRECTION ( 'NONE',  ( -1.000000000000000000, -0.000000000000000000, -0.000000000000000000 ) ) ;
#1830 = AXIS2_PLACEMENT_3D ( 'NONE', #516, #7265, #738 ) ;
#1831 = ORIENTED_EDGE ( 'NONE', *, *, #4588, .T. ) ;
#1832 = CARTESIAN_POINT ( 'NONE',  ( 10.00000000000000000, 43.18649929580291058, -73.28107340219372645 ) ) ;
#1833 = ORIENTED_EDGE ( 'NONE', *, *, #2176, .T. ) ;
#1834 = DIRECTION ( 'NONE',  ( 0.000000000000000000, 0.9510565162951521989, 0.3090169943749514481 ) ) ;
#1835 = FACE_OUTER_BOUND ( 'NONE', #9879, .T. ) ;
#1836 = ORIENTED_EDGE ( 'NONE', *, *, #16622, .F. ) ;
#1837 = DIRECTION ( 'NONE',  ( -1.000000000000000000, 0.000000000000000000, -0.000000000000000000 ) ) ;
#1838 = CIRCLE ( 'NONE', #14174, 44.99999999999999289 ) ;
#1839 = ORIENTED_EDGE ( 'NONE', *, *, #9862, .T. ) ;
#1840 = VERTEX_POINT ( 'NONE', #16823 ) ;
#1841 = VERTEX_POINT ( 'NONE', #7205 ) ;
#1842 = DIRECTION ( 'NONE',  ( -1.000000000000000000, -0.000000000000000000, -0.000000000000000000 ) ) ;
#1843 = VERTEX_POINT ( 'NONE', #362 ) ;
#1844 = DIRECTION ( 'NONE',  ( -1.000000000000000000, -0.000000000000000000, -0.000000000000000000 ) ) ;
#1845 = CARTESIAN_POINT ( 'NONE',  ( -126.5000000000000000, 1.549178200921401833E-14, -3.000000000000000000 ) ) ;
#1846 = CARTESIAN_POINT ( 'NONE',  ( 5.000000000000000000, 65.83713140174806711, -58.39068529131128571 ) ) ;
#1847 = DIRECTION ( 'NONE',  ( 0.000000000000000000, 0.000000000000000000, 1.000000000000000000 ) ) ;
#1848 = VECTOR ( 'NONE', #6161, 1000.000000000000000 ) ;
#1849 = FACE_OUTER_BOUND ( 'NONE', #12378, .T. ) ;
#1850 = CIRCLE ( 'NONE', #9585, 44.99999999999999289 ) ;
#1851 = CARTESIAN_POINT ( 'NONE',  ( 5.000000000000002665, 85.22372865846323009, -21.92979875759543162 ) ) ;
#1852 = DIRECTION ( 'NONE',  ( -1.000000000000000000, -0.000000000000000000, -0.000000000000000000 ) ) ;
#1853 = DIRECTION ( 'NONE',  ( -1.000000000000000000, -0.000000000000000000, -0.000000000000000000 ) ) ;
#1854 = AXIS2_PLACEMENT_3D ( 'NONE', #13252, #1659, #20001 ) ;
#1855 = DIRECTION ( 'NONE',  ( 0.000000000000000000, 0.000000000000000000, -1.000000000000000000 ) ) ;
#1856 = AXIS2_PLACEMENT_3D ( 'NONE', #9918, #8058, #10136 ) ;
#1857 = DIRECTION ( 'NONE',  ( 0.000000000000000000, 0.000000000000000000, 1.000000000000000000 ) ) ;
#1858 = ORIENTED_EDGE ( 'NONE', *, *, #6956, .T. ) ;
#1859 = ORIENTED_EDGE ( 'NONE', *, *, #18834, .T. ) ;
#1860 = DIRECTION ( 'NONE',  ( -1.000000000000000000, 0.000000000000000000, 0.000000000000000000 ) ) ;
#1861 = EDGE_LOOP ( 'NONE', ( #12412, #8285, #1711, #157 ) ) ;
#1862 = AXIS2_PLACEMENT_3D ( 'NONE', #6857, #11711, #6647 ) ;
#1863 = ORIENTED_EDGE ( 'NONE', *, *, #19036, .T. ) ;
#1864 = EDGE_CURVE ( 'NONE', #15501, #9734, #13526, .T. ) ;
#1865 = VERTEX_POINT ( 'NONE', #18807 ) ;
#1866 = FACE_OUTER_BOUND ( 'NONE', #5528, .T. ) ;
#1867 = ORIENTED_EDGE ( 'NONE', *, *, #18226, .T. ) ;
#1868 = CARTESIAN_POINT ( 'NONE',  ( 10.00000000000000000, 0.000000000000000000, -1.000000000000000000 ) ) ;
#1869 = DIRECTION ( 'NONE',  ( 1.000000000000000000, 0.000000000000000000, 0.000000000000000000 ) ) ;
#1870 = EDGE_CURVE ( 'NONE', #12371, #16840, #11579, .T. ) ;
#1871 = CIRCLE ( 'NONE', #14212, 2.799999999999996714 ) ;
#1872 = DIRECTION ( 'NONE',  ( -1.000000000000000000, 0.000000000000000000, 0.000000000000000000 ) ) ;
#1873 = CIRCLE ( 'NONE', #19870, 44.99999999999999289 ) ;
#1874 = DIRECTION ( 'NONE',  ( 1.000000000000000000, 0.000000000000000000, 0.000000000000000000 ) ) ;
#1875 = CARTESIAN_POINT ( 'NONE',  ( -1.114300000000000290, 0.000000000000000000, 0.000000000000000000 ) ) ;
#1876 = CARTESIAN_POINT ( 'NONE',  ( 0.000000000000000000, 5.000000000000000000, 100.0000000000000000 ) ) ;
#1877 = VECTOR ( 'NONE', #2746, 1000.000000000000000 ) ;
#1878 = ORIENTED_EDGE ( 'NONE', *, *, #7342, .F. ) ;
#1879 = FACE_OUTER_BOUND ( 'NONE', #11836, .T. ) ;
#1880 = CIRCLE ( 'NONE', #1121, 32.00000000000000000 ) ;
#1881 = ORIENTED_EDGE ( 'NONE', *, *, #11741, .T. ) ;
#1882 = VECTOR ( 'NONE', #9616, 1000.000000000000000 ) ;
#1883 = ORIENTED_EDGE ( 'NONE', *, *, #10525, .F. ) ;
#1884 = CARTESIAN_POINT ( 'NONE',  ( 0.000000000000000000, -68.93609746931124960, -54.69748134696530428 ) ) ;
#1885 = EDGE_LOOP ( 'NONE', ( #18750, #1626, #20193, #3850 ) ) ;
#1886 = EDGE_CURVE ( 'NONE', #11372, #569, #8748, .T. ) ;
#1887 = EDGE_CURVE ( 'NONE', #5459, #12003, #5582, .T. ) ;
#1888 = EDGE_CURVE ( 'NONE', #7717, #19310, #987, .T. ) ;
#1889 = VERTEX_POINT ( 'NONE', #18919 ) ;
#1890 = ORIENTED_EDGE ( 'NONE', *, *, #9749, .T. ) ;
#1891 = CARTESIAN_POINT ( 'NONE',  ( 10.00000000000000000, 0.000000000000000000, 0.000000000000000000 ) ) ;
#1892 = EDGE_CURVE ( 'NONE', #2943, #17734, #12277, .T. ) ;
#1893 = AXIS2_PLACEMENT_3D ( 'NONE', #12875, #19624, #5709 ) ;
#1894 = ORIENTED_EDGE ( 'NONE', *, *, #1993, .T. ) ;
#1895 = CARTESIAN_POINT ( 'NONE',  ( 10.00000000000000000, 84.19736439813857487, -38.30455363800848545 ) ) ;
#1896 = AXIS2_PLACEMENT_3D ( 'NONE', #15054, #11853, #13401 ) ;
#1897 = LINE ( 'NONE', #18596, #15716 ) ;
#1898 = CARTESIAN_POINT ( 'NONE',  ( 10.00000000000000000, -52.96496548042809138, -66.55750800669412115 ) ) ;
#1899 = CYLINDRICAL_SURFACE ( 'NONE', #4108, 92.50100000000000477 ) ;
#1900 = AXIS2_PLACEMENT_3D ( 'NONE', #21169, #14639, #11548 ) ;
#1901 = DIRECTION ( 'NONE',  ( 1.000000000000000000, 0.000000000000000000, 0.000000000000000000 ) ) ;
#1902 = CARTESIAN_POINT ( 'NONE',  ( 0.000000000000000000, -8.134922360105496963, -84.67002113262489615 ) ) ;
#1903 = ADVANCED_FACE ( 'NONE', ( #15160 ), #6885, .F. ) ;
#1904 = CYLINDRICAL_SURFACE ( 'NONE', #11934, 92.50100000000000477 ) ;
#1905 = ORIENTED_EDGE ( 'NONE', *, *, #5553, .T. ) ;
#1906 = EDGE_CURVE ( 'NONE', #4702, #11578, #4874, .T. ) ;
#1907 = AXIS2_PLACEMENT_3D ( 'NONE', #1492, #6482, #11557 ) ;
#1908 = CARTESIAN_POINT ( 'NONE',  ( 10.00000000000000000, 37.96946988134275358, -76.11510229470822253 ) ) ;
#1909 = DIRECTION ( 'NONE',  ( 0.000000000000000000, 0.000000000000000000, -1.000000000000000000 ) ) ;
#1910 = ORIENTED_EDGE ( 'NONE', *, *, #7365, .F. ) ;
#1911 = DIRECTION ( 'NONE',  ( 1.000000000000000000, 0.000000000000000000, 0.000000000000000000 ) ) ;
#1912 = EDGE_LOOP ( 'NONE', ( #19167, #17868, #13333, #2266 ) ) ;
#1913 = AXIS2_PLACEMENT_3D ( 'NONE', #483, #4010, #17614 ) ;
#1914 = SHAPE_REPRESENTATION_RELATIONSHIP ( 'NONE' , 'NONE' ,  #4577, #5094 ) ;
#1915 = ORIENTED_EDGE ( 'NONE', *, *, #5042, .T. ) ;
#1916 = CARTESIAN_POINT ( 'NONE',  ( 0.000000000000000000, 71.72924546250010280, -45.71766382684594276 ) ) ;
#1917 = EDGE_CURVE ( 'NONE', #18043, #1449, #33, .T. ) ;
#1918 = ORIENTED_EDGE ( 'NONE', *, *, #5142, .F. ) ;
#1919 = EDGE_LOOP ( 'NONE', ( #8029, #15366 ) ) ;
#1920 = DIRECTION ( 'NONE',  ( -1.000000000000000000, 0.000000000000000000, -0.000000000000000000 ) ) ;
#1921 = LINE ( 'NONE', #8873, #16783 ) ;
#1922 = CIRCLE ( 'NONE', #11450, 11.99999999999999645 ) ;
#1923 = DIRECTION ( 'NONE',  ( 0.000000000000000000, 0.000000000000000000, -1.000000000000000000 ) ) ;
#1924 = CYLINDRICAL_SURFACE ( 'NONE', #14695, 88.00000000000000000 ) ;
#1925 = AXIS2_PLACEMENT_3D ( 'NONE', #16639, #11882, #5363 ) ;
#1926 = CARTESIAN_POINT ( 'NONE',  ( 0.000000000000000000, -74.74361964203257003, 40.60271866773520344 ) ) ;
#1927 = CARTESIAN_POINT ( 'NONE',  ( 10.00000000000000000, -17.70753755129051754, 21.03896658273966480 ) ) ;
#1928 = CARTESIAN_POINT ( 'NONE',  ( 0.000000000000000000, 14.02138820414913845, 83.89630571862289798 ) ) ;
#1929 = DIRECTION ( 'NONE',  ( -1.000000000000000000, 0.000000000000000000, 0.000000000000000000 ) ) ;
#1930 = EDGE_CURVE ( 'NONE', #17767, #10255, #6654, .T. ) ;
#1931 = AXIS2_PLACEMENT_3D ( 'NONE', #20709, #15847, #598 ) ;
#1932 = ORIENTED_EDGE ( 'NONE', *, *, #19995, .T. ) ;
#1933 = EDGE_CURVE ( 'NONE', #9325, #12372, #20755, .T. ) ;
#1934 = VECTOR ( 'NONE', #7608, 1000.000000000000000 ) ;
#1935 = DIRECTION ( 'NONE',  ( -1.000000000000000000, -0.000000000000000000, 0.000000000000000000 ) ) ;
#1936 = FACE_OUTER_BOUND ( 'NONE', #262, .T. ) ;
#1937 = EDGE_LOOP ( 'NONE', ( #16405, #7438, #14750, #2350 ) ) ;
#1938 = ADVANCED_FACE ( 'NONE', ( #10190 ), #18597, .T. ) ;
#1939 = EDGE_CURVE ( 'NONE', #1529, #21817, #15815, .T. ) ;
#1940 = CARTESIAN_POINT ( 'NONE',  ( 10.00000000000000000, 57.47876254627226444, -62.70072803846332476 ) ) ;
#1941 = ORIENTED_EDGE ( 'NONE', *, *, #9162, .F. ) ;
#1942 = AXIS2_PLACEMENT_3D ( 'NONE', #760, #2523, #14236 ) ;
#1943 =( NAMED_UNIT ( * ) PLANE_ANGLE_UNIT ( ) SI_UNIT ( $, .RADIAN. ) );
#1944 = TOROIDAL_SURFACE ( 'NONE', #4051, 114.9007999999999896, 0.2042000000000016025 ) ;
#1945 = CARTESIAN_POINT ( 'NONE',  ( -90.00000000000000000, 0.000000000000000000, 0.000000000000000000 ) ) ;
#1946 = ORIENTED_EDGE ( 'NONE', *, *, #19010, .T. ) ;
#1947 = AXIS2_PLACEMENT_3D ( 'NONE', #12432, #11224, #4489 ) ;
#1948 = CIRCLE ( 'NONE', #10754, 114.9007999999999896 ) ;
#1949 = EDGE_LOOP ( 'NONE', ( #11976, #18648, #13217, #8141 ) ) ;
#1950 = EDGE_LOOP ( 'NONE', ( #5973, #17634, #5714, #2466 ) ) ;
#1951 = ORIENTED_EDGE ( 'NONE', *, *, #3908, .F. ) ;
#1952 = DIRECTION ( 'NONE',  ( 0.000000000000000000, 0.000000000000000000, -1.000000000000000000 ) ) ;
#1953 = AXIS2_PLACEMENT_3D ( 'NONE', #11348, #18100, #21626 ) ;
#1954 = ORIENTED_EDGE ( 'NONE', *, *, #4616, .T. ) ;
#1955 = CARTESIAN_POINT ( 'NONE',  ( -10.00000000000000000, 0.000000000000000000, 0.000000000000000000 ) ) ;
#1956 = LINE ( 'NONE', #8696, #20967 ) ;
#1957 = CYLINDRICAL_SURFACE ( 'NONE', #9804, 92.50100000000000477 ) ;
#1958 = DIRECTION ( 'NONE',  ( 1.000000000000000000, 0.000000000000000000, 0.000000000000000000 ) ) ;
#1959 = CLOSED_SHELL ( 'NONE', ( #15510, #15926, #19174, #21610, #17084, #10169, #8327, #20565, #19329, #17150, #326, #12725, #11223, #3786, #1803, #17987, #14034, #20, #14191, #10830, #7129, #9588, #18112, #311, #12383, #2698, #16095, #7831, #18003, #18664, #21235, #6920, #19178, #1343, #16660, #2982, #15138, #9090, #17035, #10135, #200, #13822, #1903, #13505, #4378, #12040, #4788, #10844, #17378, #5179, #6893, #12784, #15464, #5145, #1094, #7623, #435, #5010, #13378, #4196, #2066, #4754, #16087, #11922, #5007, #14274, #20399, #2055, #12689, #20314, #17613, #9936, #5860, #17968, #4463, #12931, #20727, #15396, #15404, #14366, #21216, #10038, #17065, #2686, #11366, #5151, #2147, #9857, #19764, #15224, #7523, #20568, #1392, #17463, #10767, #14767, #13908, #7695, #12343, #13266, #5414, #16083, #19547, #19878, #10981, #13652, #18823, #7200, #12775, #814, #19777, #19462, #2045, #10953, #11762, #11994, #15707, #15126, #5297, #15145, #16777, #19575, #13005, #10291, #10247, #1670, #7176, #7749, #18391, #14982, #13506, #8116, #14514, #1672, #6926, #10992, #17162, #1405, #4722, #19107, #5237, #7183, #14438, #11337, #1081, #10937, #2602, #18111, #21293, #1135, #20536, #1489, #9901, #6074, #4637, #2726, #8113, #11206, #10566, #6243, #15965, #21384, #10956, #18303, #15378, #12165, #653, #14883, #3909, #14908, #8982, #7072, #21579, #21482, #10666, #7024, #15973, #11774, #17452, #2934, #19742, #20134, #15280, #2857, #6018, #2061, #6769, #10662, #14163, #9084, #20848, #11321, #4383, #6121, #7966, #5615, #148, #8439, #12542, #17974, #20394, #14835, #12119, #9185, #19071, #4589, #4631, #15264, #19380, #9989, #5581, #5511, #19224, #18387, #19899, #21514, #13796, #17483, #3635, #11532, #14353, #9872, #727, #13362, #9532, #534, #19301, #20694, #18109, #3789, #20180, #9554, #17881, #14494, #5292, #13364, #15200, #18933, #4908, #21773, #17670, #6652, #12962, #20931, #21100, #15583, #7453, #18924, #20692, #9682, #18938, #15028, #16232, #1817, #6263, #1092, #11626, #16509, #8397, #20258, #19862, #18156, #13812, #7077, #14407, #21098, #2359, #17780, #16334, #16329, #5579, #3490, #11058, #14284, #18260, #986, #17811, #14183, #11868, #21047, #7708, #18804, #19887, #8207, #824, #3436, #15296, #442, #2732, #15824, #274, #12720, #1821, #15706, #5417, #14010, #17970, #4495, #2975, #18569, #17470, #21747, #18115, #3357, #2152, #12959, #11745, #4112, #3026, #7562, #8435, #10223, #10433, #10260, #13112, #11516, #19868, #12421, #4239, #12436, #18784, #11095, #21453, #9445, #9920, #6770, #11352, #2615, #18217, #12139, #9605, #7156, #16327, #17305, #6869, #19654, #10983, #16755, #5705, #14567, #8707, #3659, #5968, #8675, #10924, #15975, #14741, #3662, #281, #15809, #18619, #16113, #491, #6400, #19328, #12960, #14999, #18641, #20026, #20004, #21856, #16778, #18443, #14950, #4707, #13102, #10435 ) ) ;
#1960 = DIRECTION ( 'NONE',  ( -1.000000000000000000, 0.000000000000000000, -0.000000000000000000 ) ) ;
#1961 = CARTESIAN_POINT ( 'NONE',  ( 10.00000000000000000, 78.04699792498210797, -49.64978465107211747 ) ) ;
#1962 = CIRCLE ( 'NONE', #14297, 45.00000000000000000 ) ;
#1963 = DIRECTION ( 'NONE',  ( -1.000000000000000000, -0.000000000000000000, -0.000000000000000000 ) ) ;
#1964 = VECTOR ( 'NONE', #6052, 1000.000000000000000 ) ;
#1965 = DIRECTION ( 'NONE',  ( -0.000000000000000000, 1.000000000000000000, 0.000000000000000000 ) ) ;
#1966 = AXIS2_PLACEMENT_3D ( 'NONE', #1703, #20047, #6466 ) ;
#1967 = ORIENTED_EDGE ( 'NONE', *, *, #427, .T. ) ;
#1968 = DIRECTION ( 'NONE',  ( 0.000000000000000000, 0.000000000000000000, 1.000000000000000000 ) ) ;
#1969 = AXIS2_PLACEMENT_3D ( 'NONE', #12709, #1109, #21439 ) ;
#1970 = CARTESIAN_POINT ( 'NONE',  ( 10.00000000000000000, -27.40684453873977589, 16.51862198942000148 ) ) ;
#1971 = DIRECTION ( 'NONE',  ( 0.000000000000000000, -0.9945218953682744001, 0.1045284632676436454 ) ) ;
#1972 = VERTEX_POINT ( 'NONE', #17265 ) ;
#1973 = DIRECTION ( 'NONE',  ( 0.000000000000000000, -0.8290375725550350738, -0.5591929034707565638 ) ) ;
#1974 = VERTEX_POINT ( 'NONE', #2125 ) ;
#1975 = DIRECTION ( 'NONE',  ( 0.000000000000000000, 0.000000000000000000, 1.000000000000000000 ) ) ;
#1976 = VERTEX_POINT ( 'NONE', #8855 ) ;
#1977 = EDGE_LOOP ( 'NONE', ( #19937, #639, #18793, #17527 ) ) ;
#1978 = CIRCLE ( 'NONE', #5863, 12.00000000000000178 ) ;
#1979 = AXIS2_PLACEMENT_3D ( 'NONE', #11772, #13537, #16855 ) ;
#1980 = VECTOR ( 'NONE', #20366, 1000.000000000000000 ) ;
#1981 = EDGE_LOOP ( 'NONE', ( #7969, #21412, #17685, #15866 ) ) ;
#1982 = CIRCLE ( 'NONE', #17160, 32.00000000000000000 ) ;
#1983 = DIRECTION ( 'NONE',  ( -1.000000000000000000, 0.000000000000000000, -0.000000000000000000 ) ) ;
#1984 = ORIENTED_EDGE ( 'NONE', *, *, #13752, .F. ) ;
#1985 = CARTESIAN_POINT ( 'NONE',  ( 5.000000000000000000, -68.93609746931198856, 54.69748134696436637 ) ) ;
#1986 = DIRECTION ( 'NONE',  ( 1.000000000000000000, -0.000000000000000000, -0.000000000000000000 ) ) ;
#1987 = CARTESIAN_POINT ( 'NONE',  ( 2.000000000000000000, 67.00000000000000000, 9.999999999999998224 ) ) ;
#1988 = DIRECTION ( 'NONE',  ( 0.000000000000000000, 0.2079116908177599532, -0.9781476007338055778 ) ) ;
#1989 = CARTESIAN_POINT ( 'NONE',  ( 0.000000000000000000, 0.000000000000000000, 0.000000000000000000 ) ) ;
#1990 = FACE_OUTER_BOUND ( 'NONE', #12078, .T. ) ;
#1991 = DIRECTION ( 'NONE',  ( -1.000000000000000000, 0.000000000000000000, 0.000000000000000000 ) ) ;
#1992 = CARTESIAN_POINT ( 'NONE',  ( 10.00000000000000000, 71.72924546250010280, -45.71766382684594276 ) ) ;
#1993 = EDGE_CURVE ( 'NONE', #10561, #3324, #2405, .T. ) ;
#1994 = AXIS2_PLACEMENT_3D ( 'NONE', #4763, #3211, #21772 ) ;
#1995 = ORIENTED_EDGE ( 'NONE', *, *, #15830, .F. ) ;
#1996 = AXIS2_PLACEMENT_3D ( 'NONE', #17692, #7322, #575 ) ;
#1997 = DIRECTION ( 'NONE',  ( 0.000000000000000000, -0.9993908270190953180, -0.03489949670251103753 ) ) ;
#1998 = ORIENTED_EDGE ( 'NONE', *, *, #1508, .T. ) ;
#1999 = EDGE_CURVE ( 'NONE', #2507, #2130, #17691, .T. ) ;
#2000 = EDGE_LOOP ( 'NONE', ( #3147, #16523, #11212, #14638 ) ) ;
#2001 = DIRECTION ( 'NONE',  ( 1.000000000000000000, 0.000000000000000000, 0.000000000000000000 ) ) ;
#2002 = ORIENTED_EDGE ( 'NONE', *, *, #20917, .F. ) ;
#2003 = ORIENTED_EDGE ( 'NONE', *, *, #14233, .T. ) ;
#2004 = DIRECTION ( 'NONE',  ( -1.000000000000000000, -0.000000000000000000, -0.000000000000000000 ) ) ;
#2005 = AXIS2_PLACEMENT_3D ( 'NONE', #3206, #20013, #21442 ) ;
#2006 = AXIS2_PLACEMENT_3D ( 'NONE', #17180, #3907, #20710 ) ;
#2007 = ORIENTED_EDGE ( 'NONE', *, *, #17207, .F. ) ;
#2008 = AXIS2_PLACEMENT_3D ( 'NONE', #9253, #14356, #21101 ) ;
#2009 = CIRCLE ( 'NONE', #3083, 113.8250000000000028 ) ;
#2010 = DIRECTION ( 'NONE',  ( -1.000000000000000000, -0.000000000000000000, 0.000000000000000000 ) ) ;
#2011 = CARTESIAN_POINT ( 'NONE',  ( 10.00000000000000000, 15.32665449652044920, -91.22241316115403720 ) ) ;
#2012 = CARTESIAN_POINT ( 'NONE',  ( -1.200000000000006617, 0.000000000000000000, 0.000000000000000000 ) ) ;
#2013 = CARTESIAN_POINT ( 'NONE',  ( 5.000000000000000000, 69.74988376404090218, -53.65588238863266213 ) ) ;
#2014 = CARTESIAN_POINT ( 'NONE',  ( 0.000000000000000000, 0.000000000000000000, 0.000000000000000000 ) ) ;
#2015 = DIRECTION ( 'NONE',  ( 0.000000000000000000, 0.7431448254773953543, -0.6691306063588570163 ) ) ;
#2016 = DIRECTION ( 'NONE',  ( 0.000000000000000000, 0.000000000000000000, 1.000000000000000000 ) ) ;
#2017 = EDGE_CURVE ( 'NONE', #2438, #16240, #9383, .T. ) ;
#2018 = EDGE_CURVE ( 'NONE', #14822, #3811, #21462, .T. ) ;
#2019 = VERTEX_POINT ( 'NONE', #10726 ) ;
#2020 = CIRCLE ( 'NONE', #3782, 0.2042000000000016025 ) ;
#2021 = AXIS2_PLACEMENT_3D ( 'NONE', #17760, #12442, #11235 ) ;
#2022 = AXIS2_PLACEMENT_3D ( 'NONE', #21256, #14620, #19482 ) ;
#2023 = CARTESIAN_POINT ( 'NONE',  ( 10.00000000000000000, 12.90282758293013643, -25.06465718894764194 ) ) ;
#2024 = DIRECTION ( 'NONE',  ( 0.000000000000000000, 0.000000000000000000, 1.000000000000000000 ) ) ;
#2025 = ORIENTED_EDGE ( 'NONE', *, *, #6937, .F. ) ;
#2026 = CYLINDRICAL_SURFACE ( 'NONE', #1597, 88.00000000000000000 ) ;
#2027 = VERTEX_POINT ( 'NONE', #14046 ) ;
#2028 = EDGE_CURVE ( 'NONE', #14712, #2259, #15451, .T. ) ;
#2029 = CARTESIAN_POINT ( 'NONE',  ( 0.000000000000000000, -72.58367602204151581, -49.75550195834941292 ) ) ;
#2030 = ORIENTED_EDGE ( 'NONE', *, *, #12606, .F. ) ;
#2031 = ORIENTED_EDGE ( 'NONE', *, *, #9687, .T. ) ;
#2032 = DIRECTION ( 'NONE',  ( 0.000000000000000000, 0.000000000000000000, 1.000000000000000000 ) ) ;
#2033 = CARTESIAN_POINT ( 'NONE',  ( 1.399999999999999245, 9.062386313690440012E-16, 7.400000000000020783 ) ) ;
#2034 = EDGE_CURVE ( 'NONE', #18952, #6202, #12790, .T. ) ;
#2035 = AXIS2_PLACEMENT_3D ( 'NONE', #12161, #2004, #20784 ) ;
#2036 = FACE_OUTER_BOUND ( 'NONE', #11625, .T. ) ;
#2037 = DIRECTION ( 'NONE',  ( 0.000000000000000000, -0.6946583704589887054, -0.7193398003386594075 ) ) ;
#2038 = AXIS2_PLACEMENT_3D ( 'NONE', #14409, #21162, #6032 ) ;
#2039 = DIRECTION ( 'NONE',  ( -1.000000000000000000, 0.000000000000000000, 0.000000000000000000 ) ) ;
#2040 = AXIS2_PLACEMENT_3D ( 'NONE', #9770, #18305, #6593 ) ;
#2041 = CARTESIAN_POINT ( 'NONE',  ( 10.00000000000000000, -82.02147376274702140, 42.76579056660835221 ) ) ;
#2042 = CIRCLE ( 'NONE', #2022, 88.00000000000000000 ) ;
#2043 = CARTESIAN_POINT ( 'NONE',  ( 0.000000000000000000, -57.53593069156319473, -72.42963261301021305 ) ) ;
#2044 = DIRECTION ( 'NONE',  ( -1.000000000000000000, -0.000000000000000000, -0.000000000000000000 ) ) ;
#2045 = ADVANCED_FACE ( 'NONE', ( #11048 ), #4104, .F. ) ;
#2046 = EDGE_CURVE ( 'NONE', #21836, #16223, #2926, .T. ) ;
#2047 = ADVANCED_FACE ( 'NONE', ( #888 ), #2446, .T. ) ;
#2048 = ORIENTED_EDGE ( 'NONE', *, *, #11113, .T. ) ;
#2049 = CARTESIAN_POINT ( 'NONE',  ( 10.00000000000000000, 84.12297548659721258, -12.59025161327029529 ) ) ;
#2050 = EDGE_CURVE ( 'NONE', #447, #12668, #12486, .T. ) ;
#2051 = ORIENTED_EDGE ( 'NONE', *, *, #20131, .F. ) ;
#2052 = DIRECTION ( 'NONE',  ( 0.000000000000000000, 0.6427876096865353661, 0.7660444431189812331 ) ) ;
#2053 = ORIENTED_EDGE ( 'NONE', *, *, #13082, .F. ) ;
#2054 = AXIS2_PLACEMENT_3D ( 'NONE', #11605, #1765, #19882 ) ;
#2055 = ADVANCED_FACE ( 'NONE', ( #10946 ), #6095, .F. ) ;
#2056 = LINE ( 'NONE', #7133, #12676 ) ;
#2057 = AXIS2_PLACEMENT_3D ( 'NONE', #5448, #258, #42 ) ;
#2058 = CYLINDRICAL_SURFACE ( 'NONE', #10550, 92.50100000000000477 ) ;
#2059 = CIRCLE ( 'NONE', #12981, 7.400000000000019895 ) ;
#2060 = VERTEX_POINT ( 'NONE', #2333 ) ;
#2061 = ADVANCED_FACE ( 'NONE', ( #15919 ), #12809, .F. ) ;
#2062 = ORIENTED_EDGE ( 'NONE', *, *, #15004, .F. ) ;
#2063 = ORIENTED_EDGE ( 'NONE', *, *, #13457, .F. ) ;
#2064 = ORIENTED_EDGE ( 'NONE', *, *, #19637, .T. ) ;
#2065 = DIRECTION ( 'NONE',  ( 0.000000000000000000, 0.9271838545667883125, -0.3746065934159096833 ) ) ;
#2066 = ADVANCED_FACE ( 'NONE', ( #8957 ), #15704, .F. ) ;
#2067 = ORIENTED_EDGE ( 'NONE', *, *, #2488, .T. ) ;
#2068 = DIRECTION ( 'NONE',  ( 1.000000000000000000, 0.000000000000000000, 0.000000000000000000 ) ) ;
#2069 = DIRECTION ( 'NONE',  ( -1.000000000000000000, 0.000000000000000000, -0.000000000000000000 ) ) ;
#2070 = CYLINDRICAL_SURFACE ( 'NONE', #2752, 44.99999999999999289 ) ;
#2071 = CYLINDRICAL_SURFACE ( 'NONE', #4076, 44.99999999999999289 ) ;
#2072 = CYLINDRICAL_SURFACE ( 'NONE', #13175, 44.99999999999999289 ) ;
#2073 = ADVANCED_FACE ( 'NONE', ( #7522 ), #681, .T. ) ;
#2074 = DIRECTION ( 'NONE',  ( -1.000000000000000000, 0.000000000000000000, 0.000000000000000000 ) ) ;
#2075 = CIRCLE ( 'NONE', #19698, 5.000000000000000000 ) ;
#2076 = CARTESIAN_POINT ( 'NONE',  ( 10.00000000000000000, 0.000000000000000000, 0.000000000000000000 ) ) ;
#2077 = AXIS2_PLACEMENT_3D ( 'NONE', #1336, #14696, #6206 ) ;
#2078 = CIRCLE ( 'NONE', #2766, 45.00000000000000000 ) ;
#2079 = VERTEX_POINT ( 'NONE', #12598 ) ;
#2080 = VECTOR ( 'NONE', #688, 1000.000000000000000 ) ;
#2081 = DIRECTION ( 'NONE',  ( 1.000000000000000000, 0.000000000000000000, 0.000000000000000000 ) ) ;
#2082 = EDGE_CURVE ( 'NONE', #15909, #3420, #3984, .T. ) ;
#2083 = FACE_OUTER_BOUND ( 'NONE', #20750, .T. ) ;
#2084 = DIRECTION ( 'NONE',  ( -1.000000000000000000, 0.000000000000000000, -0.000000000000000000 ) ) ;
#2085 = ORIENTED_EDGE ( 'NONE', *, *, #4086, .F. ) ;
#2086 = DIRECTION ( 'NONE',  ( 0.000000000000000000, 1.000000000000000000, -1.224646799147353207E-16 ) ) ;
#2087 = VERTEX_POINT ( 'NONE', #16019 ) ;
#2088 = CIRCLE ( 'NONE', #16550, 11.99999999999999822 ) ;
#2089 = CARTESIAN_POINT ( 'NONE',  ( 10.00000000000000000, 0.000000000000000000, 0.000000000000000000 ) ) ;
#2090 = ORIENTED_EDGE ( 'NONE', *, *, #12151, .T. ) ;
#2091 = AXIS2_PLACEMENT_3D ( 'NONE', #7397, #21086, #17771 ) ;
#2092 = ORIENTED_EDGE ( 'NONE', *, *, #6190, .T. ) ;
#2093 = CIRCLE ( 'NONE', #13728, 92.50100000000000477 ) ;
#2094 = EDGE_CURVE ( 'NONE', #19024, #4094, #17398, .T. ) ;
#2095 = ORIENTED_EDGE ( 'NONE', *, *, #12972, .T. ) ;
#2096 = DIRECTION ( 'NONE',  ( 0.000000000000000000, 0.000000000000000000, -1.000000000000000000 ) ) ;
#2097 = DIRECTION ( 'NONE',  ( 1.000000000000000000, 0.000000000000000000, 0.000000000000000000 ) ) ;
#2098 = CYLINDRICAL_SURFACE ( 'NONE', #11036, 5.000000000000000000 ) ;
#2099 = FACE_OUTER_BOUND ( 'NONE', #1455, .T. ) ;
#2100 = EDGE_CURVE ( 'NONE', #510, #5341, #1873, .T. ) ;
#2101 = PRODUCT_DEFINITION_CONTEXT ( 'detailed design', #2331, 'design' ) ;
#2102 = CARTESIAN_POINT ( 'NONE',  ( 0.000000000000000000, 100.0000000000000000, -5.000000000000000000 ) ) ;
#2103 = DIRECTION ( 'NONE',  ( -1.000000000000000000, 0.000000000000000000, 0.000000000000000000 ) ) ;
#2104 = DIRECTION ( 'NONE',  ( 0.000000000000000000, 0.4694715627858856988, 0.8829475928589297640 ) ) ;
#2105 = DIRECTION ( 'NONE',  ( -1.000000000000000000, -0.000000000000000000, -0.000000000000000000 ) ) ;
#2106 = AXIS2_PLACEMENT_3D ( 'NONE', #12009, #10242, #8695 ) ;
#2107 = AXIS2_PLACEMENT_3D ( 'NONE', #10990, #17523, #2372 ) ;
#2108 = COLOUR_RGB ( '', 0.66274510, 0.83137255, 0.94901961) ;
#2109 = VERTEX_POINT ( 'NONE', #4756 ) ;
#2110 = CIRCLE ( 'NONE', #13743, 88.00000000000000000 ) ;
#2111 = LINE ( 'NONE', #8842, #8332 ) ;
#2112 = VERTEX_POINT ( 'NONE', #13041 ) ;
#2113 = ORIENTED_EDGE ( 'NONE', *, *, #5865, .F. ) ;
#2114 = ORIENTED_EDGE ( 'NONE', *, *, #11119, .T. ) ;
#2115 = DIRECTION ( 'NONE',  ( -1.000000000000000000, 0.000000000000000000, -0.000000000000000000 ) ) ;
#2116 = ORIENTED_EDGE ( 'NONE', *, *, #9631, .F. ) ;
#2117 = ORIENTED_EDGE ( 'NONE', *, *, #19332, .T. ) ;
#2118 = ADVANCED_FACE ( 'NONE', ( #16681 ), #4428, .T. ) ;
#2119 = DIRECTION ( 'NONE',  ( -0.000000000000000000, -0.000000000000000000, 1.000000000000000000 ) ) ;
#2120 = ORIENTED_EDGE ( 'NONE', *, *, #17838, .F. ) ;
#2121 = AXIS2_PLACEMENT_3D ( 'NONE', #6254, #9422, #19715 ) ;
#2122 = CARTESIAN_POINT ( 'NONE',  ( 0.000000000000000000, 0.000000000000000000, 0.000000000000000000 ) ) ;
#2123 = LINE ( 'NONE', #12274, #2545 ) ;
#2124 = DIRECTION ( 'NONE',  ( -1.000000000000000000, -0.000000000000000000, 0.000000000000000000 ) ) ;
#2125 = CARTESIAN_POINT ( 'NONE',  ( 0.000000000000000000, 68.93609746931237225, -54.69748134696388320 ) ) ;
#2126 = DIRECTION ( 'NONE',  ( 0.000000000000000000, 0.000000000000000000, 1.000000000000000000 ) ) ;
#2127 = DIRECTION ( 'NONE',  ( 1.000000000000000000, 0.000000000000000000, 0.000000000000000000 ) ) ;
#2128 = CARTESIAN_POINT ( 'NONE',  ( 8.899999999999987921, 0.000000000000000000, -118.9000000000000199 ) ) ;
#2129 = DIRECTION ( 'NONE',  ( 0.000000000000000000, 0.000000000000000000, 1.000000000000000000 ) ) ;
#2130 = VERTEX_POINT ( 'NONE', #19672 ) ;
#2131 = CYLINDRICAL_SURFACE ( 'NONE', #7345, 11.99999999999999645 ) ;
#2132 = DIRECTION ( 'NONE',  ( 0.000000000000000000, 0.8660254037844363761, 0.5000000000000041078 ) ) ;
#2133 = ORIENTED_EDGE ( 'NONE', *, *, #21365, .T. ) ;
#2134 = CARTESIAN_POINT ( 'NONE',  ( -10.00000000000000000, 0.000000000000000000, 0.000000000000000000 ) ) ;
#2135 = VERTEX_POINT ( 'NONE', #1548 ) ;
#2136 = CARTESIAN_POINT ( 'NONE',  ( 10.00000000000000000, 0.000000000000000000, 0.000000000000000000 ) ) ;
#2137 = ORIENTED_EDGE ( 'NONE', *, *, #6250, .T. ) ;
#2138 = EDGE_CURVE ( 'NONE', #14005, #6732, #14412, .T. ) ;
#2139 = VERTEX_POINT ( 'NONE', #12925 ) ;
#2140 = LINE ( 'NONE', #5675, #17098 ) ;
#2141 = DIRECTION ( 'NONE',  ( 1.000000000000000000, 0.000000000000000000, 0.000000000000000000 ) ) ;
#2142 = DIRECTION ( 'NONE',  ( 1.000000000000000000, -0.000000000000000000, -0.000000000000000000 ) ) ;
#2143 = CARTESIAN_POINT ( 'NONE',  ( 10.00000000000000000, -36.60317927562525853, -76.78148674856802813 ) ) ;
#2144 = DIRECTION ( 'NONE',  ( 1.000000000000000000, 0.000000000000000000, 0.000000000000000000 ) ) ;
#2145 = AXIS2_PLACEMENT_3D ( 'NONE', #2847, #9561, #14882 ) ;
#2146 = DIRECTION ( 'NONE',  ( 0.000000000000000000, 0.000000000000000000, 1.000000000000000000 ) ) ;
#2147 = ADVANCED_FACE ( 'NONE', ( #4543 ), #21655, .F. ) ;
#2148 = DIRECTION ( 'NONE',  ( 0.000000000000000000, 0.000000000000000000, -1.000000000000000000 ) ) ;
#2149 = CARTESIAN_POINT ( 'NONE',  ( 5.000000000000000000, -56.05743251323810483, -67.83483072893858434 ) ) ;
#2150 = ORIENTED_EDGE ( 'NONE', *, *, #17838, .T. ) ;
#2151 = LINE ( 'NONE', #5477, #19260 ) ;
#2152 = ADVANCED_FACE ( 'NONE', ( #4871 ), #8184, .F. ) ;
#2153 = VERTEX_POINT ( 'NONE', #21440 ) ;
#2154 = DIRECTION ( 'NONE',  ( -1.000000000000000000, -0.000000000000000000, -0.000000000000000000 ) ) ;
#2155 = VERTEX_POINT ( 'NONE', #11279 ) ;
#2156 = FACE_OUTER_BOUND ( 'NONE', #2680, .T. ) ;
#2157 = DIRECTION ( 'NONE',  ( -1.000000000000000000, 0.000000000000000000, -0.000000000000000000 ) ) ;
#2158 = ORIENTED_EDGE ( 'NONE', *, *, #422, .T. ) ;
#2160 = EDGE_CURVE ( 'NONE', #20330, #7224, #9818, .T. ) ;
#2159 = VERTEX_POINT ( 'NONE', #15321 ) ;
#2161 = ORIENTED_EDGE ( 'NONE', *, *, #18164, .T. ) ;
#2162 = EDGE_CURVE ( 'NONE', #4580, #18259, #11611, .T. ) ;
#2163 = ORIENTED_EDGE ( 'NONE', *, *, #11784, .F. ) ;
#2164 = ADVANCED_FACE ( 'NONE', ( #2775 ), #9596, .T. ) ;
#2165 = DIRECTION ( 'NONE',  ( -1.000000000000000000, 0.000000000000000000, 0.000000000000000000 ) ) ;
#2166 = VERTEX_POINT ( 'NONE', #6952 ) ;
#2167 = EDGE_CURVE ( 'NONE', #13890, #3424, #19557, .T. ) ;
#2168 = LINE ( 'NONE', #19401, #14607 ) ;
#2169 = DIRECTION ( 'NONE',  ( 0.000000000000000000, 0.000000000000000000, -1.000000000000000000 ) ) ;
#2170 = DIRECTION ( 'NONE',  ( 0.000000000000000000, 0.000000000000000000, -1.000000000000000000 ) ) ;
#2171 = LINE ( 'NONE', #2274, #5085 ) ;
#2172 = DIRECTION ( 'NONE',  ( -0.000000000000000000, -0.000000000000000000, -1.000000000000000000 ) ) ;
#2173 = DIRECTION ( 'NONE',  ( -1.000000000000000000, 0.000000000000000000, 0.000000000000000000 ) ) ;
#2174 = ORIENTED_EDGE ( 'NONE', *, *, #11312, .T. ) ;
#2175 = FACE_OUTER_BOUND ( 'NONE', #3979, .T. ) ;
#2176 = EDGE_CURVE ( 'NONE', #17490, #13354, #16467, .T. ) ;
#2177 = SHAPE_REPRESENTATION ( 'BR-820', ( #756, #15580, #9930, #1465, #413, #8871, #3942, #16283, #10279, #11706 ), #16993 ) ;
#2178 = DIRECTION ( 'NONE',  ( -1.000000000000000000, -0.000000000000000000, -0.000000000000000000 ) ) ;
#2179 = EDGE_CURVE ( 'NONE', #4068, #19613, #18317, .T. ) ;
#2180 = DIRECTION ( 'NONE',  ( 0.000000000000000000, 0.000000000000000000, 1.000000000000000000 ) ) ;
#2181 = EDGE_LOOP ( 'NONE', ( #1878, #15276, #6793, #14161 ) ) ;
#2182 = FACE_OUTER_BOUND ( 'NONE', #3133, .T. ) ;
#2183 = ORIENTED_EDGE ( 'NONE', *, *, #20898, .T. ) ;
#2184 = CYLINDRICAL_SURFACE ( 'NONE', #14053, 92.50100000000000477 ) ;
#2185 = ORIENTED_EDGE ( 'NONE', *, *, #7062, .F. ) ;
#2186 = EDGE_LOOP ( 'NONE', ( #8307, #13055, #12438, #12358 ) ) ;
#2187 = DIRECTION ( 'NONE',  ( -1.000000000000000000, -0.000000000000000000, -0.000000000000000000 ) ) ;
#2188 = EDGE_LOOP ( 'NONE', ( #16537, #1437, #1782, #15450 ) ) ;
#2189 = DIRECTION ( 'NONE',  ( -1.000000000000000000, 0.000000000000000000, -0.000000000000000000 ) ) ;
#2190 = EDGE_CURVE ( 'NONE', #18794, #6346, #11600, .T. ) ;
#2191 = AXIS2_PLACEMENT_3D ( 'NONE', #21437, #6323, #21221 ) ;
#2192 = DIRECTION ( 'NONE',  ( 0.000000000000000000, 0.000000000000000000, 1.000000000000000000 ) ) ;
#2193 = LINE ( 'NONE', #5735, #4339 ) ;
#2194 = SURFACE_SIDE_STYLE ('',( #3536 ) ) ;
#2195 = CARTESIAN_POINT ( 'NONE',  ( 0.000000000000000000, 65.64563793391906188, -54.09103124042745492 ) ) ;
#2196 = DIRECTION ( 'NONE',  ( -1.000000000000000000, -0.000000000000000000, -0.000000000000000000 ) ) ;
#2197 = DIRECTION ( 'NONE',  ( -0.000000000000000000, 1.000000000000000000, 0.000000000000000000 ) ) ;
#2198 = DIRECTION ( 'NONE',  ( 0.000000000000000000, 0.9945218953682736229, -0.1045284632676503761 ) ) ;
#2199 = CARTESIAN_POINT ( 'NONE',  ( 10.00000000000000000, 85.22372865846323009, -21.92979875759543162 ) ) ;
#2200 = EDGE_CURVE ( 'NONE', #17790, #1295, #9739, .T. ) ;
#2201 = ORIENTED_EDGE ( 'NONE', *, *, #16501, .F. ) ;
#2202 = ADVANCED_FACE ( 'NONE', ( #21553 ), #6432, .T. ) ;
#2203 = DIRECTION ( 'NONE',  ( 1.000000000000000000, 0.000000000000000000, 0.000000000000000000 ) ) ;
#2204 = EDGE_LOOP ( 'NONE', ( #14119, #4888, #21368, #5020 ) ) ;
#2205 = AXIS2_PLACEMENT_3D ( 'NONE', #11819, #16463, #15230 ) ;
#2206 = ORIENTED_EDGE ( 'NONE', *, *, #11511, .T. ) ;
#2207 = EDGE_CURVE ( 'NONE', #2619, #6547, #18236, .T. ) ;
#2208 = EDGE_CURVE ( 'NONE', #4047, #20991, #7057, .T. ) ;
#2209 = ORIENTED_EDGE ( 'NONE', *, *, #4224, .T. ) ;
#2210 = FACE_OUTER_BOUND ( 'NONE', #19200, .T. ) ;
#2211 = AXIS2_PLACEMENT_3D ( 'NONE', #18894, #3751, #17240 ) ;
#2212 = AXIS2_PLACEMENT_3D ( 'NONE', #224, #10595, #339 ) ;
#2213 = ORIENTED_EDGE ( 'NONE', *, *, #16340, .F. ) ;
#2214 = VERTEX_POINT ( 'NONE', #3611 ) ;
#2215 = AXIS2_PLACEMENT_3D ( 'NONE', #21202, #5964, #4404 ) ;
#2216 = DIRECTION ( 'NONE',  ( 1.000000000000000000, -0.000000000000000000, -0.000000000000000000 ) ) ;
#2217 = EDGE_LOOP ( 'NONE', ( #2814, #18602, #478, #11703 ) ) ;
#2218 = DIRECTION ( 'NONE',  ( 0.000000000000000000, 0.9510565162951544194, -0.3090169943749448977 ) ) ;
#2219 = DIRECTION ( 'NONE',  ( 0.000000000000000000, 0.000000000000000000, 1.000000000000000000 ) ) ;
#2220 = CIRCLE ( 'NONE', #12437, 44.99999999999999289 ) ;
#2221 = CARTESIAN_POINT ( 'NONE',  ( -1.500346250137462226E-14, 60.00000000000001421, 0.000000000000000000 ) ) ;
#2222 = DIRECTION ( 'NONE',  ( 0.000000000000000000, 0.000000000000000000, 1.000000000000000000 ) ) ;
#2223 = CARTESIAN_POINT ( 'NONE',  ( 0.000000000000000000, -2.208823992043557283, -85.03123271466938604 ) ) ;
#2224 = CARTESIAN_POINT ( 'NONE',  ( 10.00000000000000000, 0.000000000000000000, 0.000000000000000000 ) ) ;
#2225 = DIRECTION ( 'NONE',  ( -1.000000000000000000, 0.000000000000000000, 0.000000000000000000 ) ) ;
#2226 = DIRECTION ( 'NONE',  ( 0.000000000000000000, 0.000000000000000000, -1.000000000000000000 ) ) ;
#2227 = VECTOR ( 'NONE', #13531, 1000.000000000000000 ) ;
#2228 = AXIS2_PLACEMENT_3D ( 'NONE', #7935, #14457, #21300 ) ;
#2229 = ORIENTED_EDGE ( 'NONE', *, *, #18915, .T. ) ;
#2230 = CIRCLE ( 'NONE', #16331, 6.887500000000022382 ) ;
#2231 = CARTESIAN_POINT ( 'NONE',  ( 0.000000000000000000, -64.66851233300764079, 55.25552418572942059 ) ) ;
#2232 = DIRECTION ( 'NONE',  ( -1.000000000000000000, -0.000000000000000000, -0.000000000000000000 ) ) ;
#2233 = AXIS2_PLACEMENT_3D ( 'NONE', #1085, #9245, #6180 ) ;
#2234 = ORIENTED_EDGE ( 'NONE', *, *, #12389, .T. ) ;
#2235 = DIRECTION ( 'NONE',  ( 0.000000000000000000, 0.2756373558169932791, 0.9612616959383205595 ) ) ;
#2236 = EDGE_LOOP ( 'NONE', ( #12449, #5599, #19523, #18390 ) ) ;
#2237 =( LENGTH_UNIT ( ) NAMED_UNIT ( * ) SI_UNIT ( .MILLI., .METRE. ) );
#2238 = AXIS2_PLACEMENT_3D ( 'NONE', #19920, #1466, #14942 ) ;
#2239 = DIRECTION ( 'NONE',  ( 0.000000000000000000, 0.000000000000000000, 1.000000000000000000 ) ) ;
#2240 = VERTEX_POINT ( 'NONE', #10576 ) ;
#2241 = EDGE_LOOP ( 'NONE', ( #11968, #17439, #21457, #9613 ) ) ;
#2242 = CYLINDRICAL_SURFACE ( 'NONE', #8619, 11.99999999999999822 ) ;
#2243 = DIRECTION ( 'NONE',  ( 0.000000000000000000, 0.000000000000000000, 1.000000000000000000 ) ) ;
#2244 = AXIS2_PLACEMENT_3D ( 'NONE', #19804, #6229, #21023 ) ;
#2245 = CARTESIAN_POINT ( 'NONE',  ( 0.000000000000000000, 74.39348546125053474, 54.97312363261438151 ) ) ;
#2246 = CARTESIAN_POINT ( 'NONE',  ( 10.00000000000000000, 61.71252885873388294, 58.53847642588613809 ) ) ;
#2247 = DIRECTION ( 'NONE',  ( 0.000000000000000000, 1.000000000000000000, -1.224646799147353207E-16 ) ) ;
#2248 = DIRECTION ( 'NONE',  ( 0.000000000000000000, -0.3420201433256757073, 0.9396926207859057634 ) ) ;
#2249 = DIRECTION ( 'NONE',  ( 1.000000000000000000, 0.000000000000000000, 0.000000000000000000 ) ) ;
#2250 = DIRECTION ( 'NONE',  ( 0.000000000000000000, -0.7431448254774000173, 0.6691306063588517983 ) ) ;
#2251 = AXIS2_PLACEMENT_3D ( 'NONE', #2388, #11002, #20846 ) ;
#2252 = ORIENTED_EDGE ( 'NONE', *, *, #16247, .T. ) ;
#2253 = CARTESIAN_POINT ( 'NONE',  ( 0.000000000000000000, -91.70173545986510533, -12.13370160540135778 ) ) ;
#2254 = AXIS2_PLACEMENT_3D ( 'NONE', #12984, #9769, #1393 ) ;
#2255 = EDGE_CURVE ( 'NONE', #5950, #18176, #17099, .T. ) ;
#2256 = EDGE_LOOP ( 'NONE', ( #9104, #1580, #6007, #10175 ) ) ;
#2257 = VECTOR ( 'NONE', #16842, 1000.000000000000000 ) ;
#2258 = CARTESIAN_POINT ( 'NONE',  ( 1.399999999999998579, 9.184850993605177527E-16, 7.500000000000022204 ) ) ;
#2259 = VERTEX_POINT ( 'NONE', #3725 ) ;
#2260 = CARTESIAN_POINT ( 'NONE',  ( -10.00000000000000000, 0.000000000000000000, 0.000000000000000000 ) ) ;
#2261 = DIRECTION ( 'NONE',  ( -1.000000000000000000, 0.000000000000000000, 0.000000000000000000 ) ) ;
#2262 = VERTEX_POINT ( 'NONE', #1961 ) ;
#2263 = EDGE_CURVE ( 'NONE', #13273, #3104, #7147, .T. ) ;
#2264 = AXIS2_PLACEMENT_3D ( 'NONE', #9410, #1037, #10975 ) ;
#2265 = ORIENTED_EDGE ( 'NONE', *, *, #1533, .F. ) ;
#2266 = ORIENTED_EDGE ( 'NONE', *, *, #6042, .T. ) ;
#2267 = VERTEX_POINT ( 'NONE', #14108 ) ;
#2268 = DIRECTION ( 'NONE',  ( 1.000000000000000000, 0.000000000000000000, 0.000000000000000000 ) ) ;
#2269 = ORIENTED_EDGE ( 'NONE', *, *, #17543, .F. ) ;
#2270 = VECTOR ( 'NONE', #1283, 1000.000000000000000 ) ;
#2271 = DIRECTION ( 'NONE',  ( 0.000000000000000000, 0.9510565162951544194, -0.3090169943749450088 ) ) ;
#2272 = FACE_OUTER_BOUND ( 'NONE', #4924, .T. ) ;
#2273 = CARTESIAN_POINT ( 'NONE',  ( -1.200000000000006617, 0.000000000000000000, -6.728125000000022560 ) ) ;
#2274 = CARTESIAN_POINT ( 'NONE',  ( 10.00000000000000000, -27.87320266523496315, -88.20158487341788600 ) ) ;
#2275 = AXIS2_PLACEMENT_3D ( 'NONE', #15843, #7445, #8975 ) ;
#2276 = DIRECTION ( 'NONE',  ( 0.000000000000000000, 0.000000000000000000, -1.000000000000000000 ) ) ;
#2277 = ORIENTED_EDGE ( 'NONE', *, *, #12001, .F. ) ;
#2278 = CARTESIAN_POINT ( 'NONE',  ( 10.00000000000000000, -84.12297548659712731, -12.59025161327086906 ) ) ;
#2279 = AXIS2_PLACEMENT_3D ( 'NONE', #11304, #20344, #13169 ) ;
#2280 = CARTESIAN_POINT ( 'NONE',  ( -8.900000000000018119, 0.000000000000000000, 0.000000000000000000 ) ) ;
#2281 = EDGE_CURVE ( 'NONE', #1054, #6321, #8703, .T. ) ;
#2283 = EDGE_CURVE ( 'NONE', #21012, #3811, #18978, .T. ) ;
#2282 = CIRCLE ( 'NONE', #8291, 92.50100000000000477 ) ;
#2284 = ADVANCED_FACE ( 'NONE', ( #8704 ), #17538, .F. ) ;
#2285 = CIRCLE ( 'NONE', #7288, 44.99999999999998579 ) ;
#2286 = CARTESIAN_POINT ( 'NONE',  ( 0.000000000000000000, -87.96697768756401103, -2.410567674971490604 ) ) ;
#2287 = AXIS2_PLACEMENT_3D ( 'NONE', #12951, #7778, #19589 ) ;
#2288 = VERTEX_POINT ( 'NONE', #10462 ) ;
#2289 = ADVANCED_FACE ( 'NONE', ( #7377 ), #15436, .T. ) ;
#2290 = CARTESIAN_POINT ( 'NONE',  ( -10.00000000000000000, 0.000000000000000000, 100.0000000000000000 ) ) ;
#2291 = ORIENTED_EDGE ( 'NONE', *, *, #6500, .F. ) ;
#2292 = CARTESIAN_POINT ( 'NONE',  ( 0.000000000000000000, 0.000000000000000000, 0.000000000000000000 ) ) ;
#2293 = VECTOR ( 'NONE', #18270, 1000.000000000000000 ) ;
#2294 = VERTEX_POINT ( 'NONE', #13879 ) ;
#2295 = ORIENTED_EDGE ( 'NONE', *, *, #12743, .T. ) ;
#2296 = ORIENTED_EDGE ( 'NONE', *, *, #8034, .T. ) ;
#2297 = CARTESIAN_POINT ( 'NONE',  ( 10.00000000000000000, 0.000000000000000000, 0.000000000000000000 ) ) ;
#2298 = EDGE_LOOP ( 'NONE', ( #10010, #1946, #18590, #12079 ) ) ;
#2299 = EDGE_CURVE ( 'NONE', #8019, #6618, #4822, .T. ) ;
#2300 = DIRECTION ( 'NONE',  ( 0.000000000000000000, 0.000000000000000000, 1.000000000000000000 ) ) ;
#2301 = CARTESIAN_POINT ( 'NONE',  ( -90.00000000000000000, 8.434754829127421589E-16, 6.887500000000022382 ) ) ;
#2302 = LINE ( 'NONE', #15566, #2548 ) ;
#2303 = AXIS2_PLACEMENT_3D ( 'NONE', #21284, #11006, #632 ) ;
#2304 = AXIS2_PLACEMENT_3D ( 'NONE', #13626, #17053, #15604 ) ;
#2305 = CYLINDRICAL_SURFACE ( 'NONE', #2561, 11.99999999999999822 ) ;
#2306 = VECTOR ( 'NONE', #16526, 1000.000000000000000 ) ;
#2307 = EDGE_CURVE ( 'NONE', #18181, #13603, #17004, .T. ) ;
#2308 = FACE_OUTER_BOUND ( 'NONE', #119, .T. ) ;
#2309 = FACE_OUTER_BOUND ( 'NONE', #5727, .T. ) ;
#2310 = DIRECTION ( 'NONE',  ( 1.000000000000000000, 0.000000000000000000, 0.000000000000000000 ) ) ;
#2311 = LINE ( 'NONE', #5744, #2728 ) ;
#2312 = CARTESIAN_POINT ( 'NONE',  ( 0.000000000000000000, 0.000000000000000000, 0.000000000000000000 ) ) ;
#2313 = EDGE_CURVE ( 'NONE', #8737, #9671, #17322, .T. ) ;
#2314 = ORIENTED_EDGE ( 'NONE', *, *, #5454, .T. ) ;
#2315 = CYLINDRICAL_SURFACE ( 'NONE', #18232, 10.49999999999999822 ) ;
#2316 = ORIENTED_EDGE ( 'NONE', *, *, #18957, .F. ) ;
#2317 = EDGE_CURVE ( 'NONE', #6258, #13543, #66, .T. ) ;
#2318 = ORIENTED_EDGE ( 'NONE', *, *, #1463, .F. ) ;
#2319 = CIRCLE ( 'NONE', #15327, 44.99999999999998579 ) ;
#2320 = ORIENTED_EDGE ( 'NONE', *, *, #3783, .F. ) ;
#2321 = DIRECTION ( 'NONE',  ( 0.000000000000000000, 0.000000000000000000, 1.000000000000000000 ) ) ;
#2322 = ORIENTED_EDGE ( 'NONE', *, *, #1654, .F. ) ;
#2323 = ORIENTED_EDGE ( 'NONE', *, *, #14471, .F. ) ;
#2324 = ORIENTED_EDGE ( 'NONE', *, *, #1375, .T. ) ;
#2325 = EDGE_CURVE ( 'NONE', #17111, #5399, #19819, .T. ) ;
#2326 = CARTESIAN_POINT ( 'NONE',  ( -10.00000000000000000, 0.000000000000000000, 0.000000000000000000 ) ) ;
#2327 = ORIENTED_EDGE ( 'NONE', *, *, #18525, .F. ) ;
#2328 = EDGE_CURVE ( 'NONE', #15305, #18649, #12398, .T. ) ;
#2329 = DIRECTION ( 'NONE',  ( 0.000000000000000000, 0.000000000000000000, 1.000000000000000000 ) ) ;
#2330 = CARTESIAN_POINT ( 'NONE',  ( 0.000000000000000000, 3.786343810537937227, -27.23708136986048700 ) ) ;
#2331 = APPLICATION_CONTEXT ( 'automotive_design' ) ;
#2332 = FACE_OUTER_BOUND ( 'NONE', #3263, .T. ) ;
#2333 = CARTESIAN_POINT ( 'NONE',  ( 10.49999999999999822, 1.285879139104720633E-15, 3.000000000000000000 ) ) ;
#2334 = CARTESIAN_POINT ( 'NONE',  ( -10.00000000000001243, 0.000000000000000000, -101.1000000000000369 ) ) ;
#2335 = EDGE_CURVE ( 'NONE', #6010, #20772, #5712, .T. ) ;
#2336 = VECTOR ( 'NONE', #3665, 1000.000000000000000 ) ;
#2337 = EDGE_CURVE ( 'NONE', #2883, #17333, #13995, .T. ) ;
#2338 = DIRECTION ( 'NONE',  ( 0.000000000000000000, -0.4694715627858974116, 0.8829475928589234357 ) ) ;
#2339 = CARTESIAN_POINT ( 'NONE',  ( 10.00000000000000000, -81.32027326007839463, -44.08455690949136851 ) ) ;
#2340 = DIRECTION ( 'NONE',  ( 0.000000000000000000, -0.7431448254773861395, -0.6691306063588671194 ) ) ;
#2341 = ORIENTED_EDGE ( 'NONE', *, *, #1654, .T. ) ;
#2342 = CARTESIAN_POINT ( 'NONE',  ( -90.00000000000000000, 0.000000000000000000, 0.000000000000000000 ) ) ;
#2343 = EDGE_CURVE ( 'NONE', #5948, #1656, #20876, .T. ) ;
#2344 = LINE ( 'NONE', #11062, #17237 ) ;
#2345 = CYLINDRICAL_SURFACE ( 'NONE', #15877, 44.99999999999999289 ) ;
#2346 = CIRCLE ( 'NONE', #11535, 45.00000000000000000 ) ;
#2347 = ORIENTED_EDGE ( 'NONE', *, *, #18669, .F. ) ;
#2348 = CIRCLE ( 'NONE', #20361, 44.99999999999998579 ) ;
#2349 = CARTESIAN_POINT ( 'NONE',  ( 5.000000000000002665, -86.54587337002888603, 15.93147207946976707 ) ) ;
#2350 = ORIENTED_EDGE ( 'NONE', *, *, #19282, .T. ) ;
#2351 = CARTESIAN_POINT ( 'NONE',  ( 0.000000000000000000, 51.76708072107978609, -67.49339815138442589 ) ) ;
#2352 = ORIENTED_EDGE ( 'NONE', *, *, #15535, .T. ) ;
#2353 = ORIENTED_EDGE ( 'NONE', *, *, #20965, .T. ) ;
#2354 = CARTESIAN_POINT ( 'NONE',  ( 10.00000000000000000, -62.44821182181044605, -68.23969402963567177 ) ) ;
#2355 = CYLINDRICAL_SURFACE ( 'NONE', #20987, 88.00000000000000000 ) ;
#2356 = CYLINDRICAL_SURFACE ( 'NONE', #9447, 27.49900000000000233 ) ;
#2357 = DIRECTION ( 'NONE',  ( -1.000000000000000000, -0.000000000000000000, -0.000000000000000000 ) ) ;
#2358 = DIRECTION ( 'NONE',  ( 0.000000000000000000, 0.4694715627858856988, 0.8829475928589297640 ) ) ;
#2359 = ADVANCED_FACE ( 'NONE', ( #5711 ), #9011, .F. ) ;
#2360 = DIRECTION ( 'NONE',  ( 1.000000000000000000, 0.000000000000000000, 0.000000000000000000 ) ) ;
#2361 = DIRECTION ( 'NONE',  ( 0.000000000000000000, -0.9510565162951566398, 0.3090169943749382364 ) ) ;
#2362 = FACE_OUTER_BOUND ( 'NONE', #15065, .T. ) ;
#2363 = TOROIDAL_SURFACE ( 'NONE', #18246, 6.866799999999992465, 0.02570000000000154800 ) ;
#2364 = AXIS2_PLACEMENT_3D ( 'NONE', #1615, #15086, #13103 ) ;
#2365 = ORIENTED_EDGE ( 'NONE', *, *, #14355, .T. ) ;
#2366 = VECTOR ( 'NONE', #15346, 1000.000000000000000 ) ;
#2367 = DIRECTION ( 'NONE',  ( -1.000000000000000000, -0.000000000000000000, -0.000000000000000000 ) ) ;
#2368 = ORIENTED_EDGE ( 'NONE', *, *, #19445, .T. ) ;
#2369 = FACE_OUTER_BOUND ( 'NONE', #704, .T. ) ;
#2370 = EDGE_LOOP ( 'NONE', ( #1833, #5367, #4927, #13954 ) ) ;
#2371 = CARTESIAN_POINT ( 'NONE',  ( 0.000000000000000000, 0.000000000000000000, 3.000000000000000000 ) ) ;
#2372 = DIRECTION ( 'NONE',  ( 0.000000000000000000, 0.000000000000000000, 1.000000000000000000 ) ) ;
#2373 = ORIENTED_EDGE ( 'NONE', *, *, #11742, .T. ) ;
#2374 = SURFACE_STYLE_USAGE ( .BOTH. , #7253 ) ;
#2375 = ORIENTED_EDGE ( 'NONE', *, *, #21568, .F. ) ;
#2376 = ORIENTED_EDGE ( 'NONE', *, *, #3937, .T. ) ;
#2377 = CIRCLE ( 'NONE', #7329, 7.500000000000000000 ) ;
#2378 = VERTEX_POINT ( 'NONE', #21177 ) ;
#2379 = DIRECTION ( 'NONE',  ( 0.000000000000000000, 0.000000000000000000, 1.000000000000000000 ) ) ;
#2380 = DIRECTION ( 'NONE',  ( 0.000000000000000000, -0.4067366430758070917, 0.9135454576425977580 ) ) ;
#2381 = VECTOR ( 'NONE', #6129, 1000.000000000000000 ) ;
#2382 = EDGE_CURVE ( 'NONE', #1056, #17052, #1376, .T. ) ;
#2383 = ORIENTED_EDGE ( 'NONE', *, *, #4759, .F. ) ;
#2384 = CARTESIAN_POINT ( 'NONE',  ( 5.000000000000000000, 86.54587337002878655, 15.93147207947034971 ) ) ;
#2385 = CARTESIAN_POINT ( 'NONE',  ( -10.00000000000000000, 0.000000000000000000, 0.000000000000000000 ) ) ;
#2386 = EDGE_CURVE ( 'NONE', #1656, #6035, #19625, .T. ) ;
#2387 = CARTESIAN_POINT ( 'NONE',  ( 10.00000000000000000, -56.35896156214896280, -73.34918167666369015 ) ) ;
#2388 = CARTESIAN_POINT ( 'NONE',  ( 10.00000000000000000, -81.55207211302094095, 24.17537951050038814 ) ) ;
#2389 = DIRECTION ( 'NONE',  ( -1.000000000000000000, -0.000000000000000000, -0.000000000000000000 ) ) ;
#2390 = ORIENTED_EDGE ( 'NONE', *, *, #18284, .T. ) ;
#2391 = EDGE_CURVE ( 'NONE', #6398, #12588, #5257, .T. ) ;
#2392 = CARTESIAN_POINT ( 'NONE',  ( 10.00000000000000000, -22.77465461094683974, 15.41136296218079238 ) ) ;
#2393 = AXIS2_PLACEMENT_3D ( 'NONE', #4154, #10887, #14311 ) ;
#2394 = AXIS2_PLACEMENT_3D ( 'NONE', #7779, #10972, #7344 ) ;
#2395 = CARTESIAN_POINT ( 'NONE',  ( 10.00000000000000888, 0.000000000000000000, 3.000000000000000444 ) ) ;
#2396 = AXIS2_PLACEMENT_3D ( 'NONE', #2023, #20482, #7216 ) ;
#2397 = CIRCLE ( 'NONE', #8059, 32.00000000000000000 ) ;
#2398 = CIRCLE ( 'NONE', #16522, 27.49900000000000233 ) ;
#2399 = CARTESIAN_POINT ( 'NONE',  ( 10.00000000000000000, -85.22372865846278955, -21.92979875759713693 ) ) ;
#2400 = ORIENTED_EDGE ( 'NONE', *, *, #7207, .F. ) ;
#2401 = DIRECTION ( 'NONE',  ( 0.000000000000000000, -0.8987940462991618196, -0.4383711467890877289 ) ) ;
#2402 = EDGE_LOOP ( 'NONE', ( #14186, #5487, #1077, #20352 ) ) ;
#2403 = CARTESIAN_POINT ( 'NONE',  ( 0.000000000000000000, 0.000000000000000000, 0.000000000000000000 ) ) ;
#2404 = ORIENTED_EDGE ( 'NONE', *, *, #13422, .T. ) ;
#2405 = CIRCLE ( 'NONE', #283, 88.00000000000000000 ) ;
#2406 = ORIENTED_EDGE ( 'NONE', *, *, #13279, .F. ) ;
#2407 = ORIENTED_EDGE ( 'NONE', *, *, #5738, .T. ) ;
#2408 = DIRECTION ( 'NONE',  ( -1.000000000000000000, -0.000000000000000000, -0.000000000000000000 ) ) ;
#2409 = ORIENTED_EDGE ( 'NONE', *, *, #21341, .F. ) ;
#2410 = DIRECTION ( 'NONE',  ( 1.000000000000000000, 0.000000000000000000, 0.000000000000000000 ) ) ;
#2411 = VECTOR ( 'NONE', #4973, 1000.000000000000000 ) ;
#2412 = CARTESIAN_POINT ( 'NONE',  ( 0.000000000000000000, 7.619321854369562885, 26.42235673590693423 ) ) ;
#2413 = DIRECTION ( 'NONE',  ( -1.000000000000000000, 0.000000000000000000, 0.000000000000000000 ) ) ;
#2414 = EDGE_CURVE ( 'NONE', #18093, #4970, #19508, .T. ) ;
#2415 = AXIS2_PLACEMENT_3D ( 'NONE', #14118, #8823, #8916 ) ;
#2416 = VECTOR ( 'NONE', #16143, 1000.000000000000000 ) ;
#2417 = CARTESIAN_POINT ( 'NONE',  ( 10.00000000000000000, -14.02138820414970688, 83.89630571862279851 ) ) ;
#2418 = DIRECTION ( 'NONE',  ( -1.000000000000000000, 0.000000000000000000, -0.000000000000000000 ) ) ;
#2419 = DIRECTION ( 'NONE',  ( -1.000000000000000000, 0.000000000000000000, 0.000000000000000000 ) ) ;
#2420 = DIRECTION ( 'NONE',  ( 0.000000000000000000, 0.000000000000000000, 1.000000000000000000 ) ) ;
#2421 = EDGE_CURVE ( 'NONE', #16693, #9876, #4907, .T. ) ;
#2422 = DIRECTION ( 'NONE',  ( 0.000000000000000000, 0.000000000000000000, 1.000000000000000000 ) ) ;
#2423 = LINE ( 'NONE', #7297, #17962 ) ;
#2424 = FACE_OUTER_BOUND ( 'NONE', #8917, .T. ) ;
#2425 = EDGE_CURVE ( 'NONE', #18297, #8691, #14429, .T. ) ;
#2426 = AXIS2_PLACEMENT_3D ( 'NONE', #11926, #2410, #14455 ) ;
#2427 = VERTEX_POINT ( 'NONE', #5826 ) ;
#2428 = AXIS2_PLACEMENT_3D ( 'NONE', #2128, #8858, #13940 ) ;
#2429 = CIRCLE ( 'NONE', #5624, 27.49900000000000233 ) ;
#2430 = ORIENTED_EDGE ( 'NONE', *, *, #4064, .F. ) ;
#2431 = AXIS2_PLACEMENT_3D ( 'NONE', #19748, #2729, #16544 ) ;
#2432 = AXIS2_PLACEMENT_3D ( 'NONE', #20986, #5858, #12581 ) ;
#2433 = ORIENTED_EDGE ( 'NONE', *, *, #1496, .F. ) ;
#2434 = VERTEX_POINT ( 'NONE', #12989 ) ;
#2435 = ORIENTED_EDGE ( 'NONE', *, *, #11948, .F. ) ;
#2436 = CARTESIAN_POINT ( 'NONE',  ( -10.00000000000000000, 0.000000000000000000, 0.000000000000000000 ) ) ;
#2437 = EDGE_CURVE ( 'NONE', #5370, #16155, #8784, .T. ) ;
#2438 = VERTEX_POINT ( 'NONE', #14648 ) ;
#2439 = EDGE_CURVE ( 'NONE', #13824, #19161, #4268, .T. ) ;
#2440 = EDGE_CURVE ( 'NONE', #21840, #6987, #13721, .T. ) ;
#2441 = LINE ( 'NONE', #7421, #20982 ) ;
#2442 = CARTESIAN_POINT ( 'NONE',  ( 10.00000000000000000, -46.93287725819829603, 70.94007663282431508 ) ) ;
#2443 = AXIS2_PLACEMENT_3D ( 'NONE', #20912, #5787, #17617 ) ;
#2444 = EDGE_CURVE ( 'NONE', #18200, #4811, #2088, .T. ) ;
#2445 = DIRECTION ( 'NONE',  ( 0.000000000000000000, 0.000000000000000000, -1.000000000000000000 ) ) ;
#2446 = CYLINDRICAL_SURFACE ( 'NONE', #6108, 32.00000000000000000 ) ;
#2447 = CIRCLE ( 'NONE', #15502, 11.99999999999999645 ) ;
#2448 = CYLINDRICAL_SURFACE ( 'NONE', #7639, 88.00000000000000000 ) ;
#2449 = CIRCLE ( 'NONE', #2803, 88.00000000000000000 ) ;
#2450 = DIRECTION ( 'NONE',  ( 0.000000000000000000, 0.000000000000000000, 1.000000000000000000 ) ) ;
#2451 = DIRECTION ( 'NONE',  ( -1.000000000000000000, -0.000000000000000000, -0.000000000000000000 ) ) ;
#2452 = FACE_OUTER_BOUND ( 'NONE', #12977, .T. ) ;
#2453 = VERTEX_POINT ( 'NONE', #11327 ) ;
#2454 = DIRECTION ( 'NONE',  ( 0.000000000000000000, 0.000000000000000000, 1.000000000000000000 ) ) ;
#2455 = EDGE_CURVE ( 'NONE', #19437, #14902, #18328, .T. ) ;
#2456 = DIRECTION ( 'NONE',  ( 1.000000000000000000, -0.000000000000000000, 0.000000000000000000 ) ) ;
#2457 = EDGE_CURVE ( 'NONE', #10255, #11426, #2604, .T. ) ;
#2458 = CARTESIAN_POINT ( 'NONE',  ( 10.00000000000000000, 92.49798535263880694, -0.7467976319023919007 ) ) ;
#2459 = ORIENTED_EDGE ( 'NONE', *, *, #14476, .T. ) ;
#2460 = CIRCLE ( 'NONE', #697, 44.99999999999999289 ) ;
#2461 = CARTESIAN_POINT ( 'NONE',  ( -1.114300000000000068, 0.000000000000000000, -5.633200000000004870 ) ) ;
#2462 = AXIS2_PLACEMENT_3D ( 'NONE', #5259, #20502, #12091 ) ;
#2463 = VERTEX_POINT ( 'NONE', #15971 ) ;
#2464 = EDGE_CURVE ( 'NONE', #18297, #2871, #12762, .T. ) ;
#2465 = DIRECTION ( 'NONE',  ( 0.000000000000000000, -0.7880107536067145757, -0.6156614753256675066 ) ) ;
#2466 = ORIENTED_EDGE ( 'NONE', *, *, #17407, .T. ) ;
#2467 = ORIENTED_EDGE ( 'NONE', *, *, #15247, .F. ) ;
#2468 = CARTESIAN_POINT ( 'NONE',  ( 0.000000000000000000, 0.000000000000000000, 0.000000000000000000 ) ) ;
#2469 = CYLINDRICAL_SURFACE ( 'NONE', #6344, 88.00000000000000000 ) ;
#2470 = EDGE_CURVE ( 'NONE', #5352, #5864, #17979, .T. ) ;
#2471 = DIRECTION ( 'NONE',  ( 0.000000000000000000, 0.000000000000000000, 1.000000000000000000 ) ) ;
#2472 = DIRECTION ( 'NONE',  ( -1.000000000000000000, -0.000000000000000000, 0.000000000000000000 ) ) ;
#2473 = CYLINDRICAL_SURFACE ( 'NONE', #21740, 44.99999999999998579 ) ;
#2474 = CARTESIAN_POINT ( 'NONE',  ( 5.000000000000002665, -76.53853822673953289, -43.42639941457193231 ) ) ;
#2475 = CARTESIAN_POINT ( 'NONE',  ( 0.000000000000000000, -92.32475887865429343, 5.707354816230212791 ) ) ;
#2476 = CARTESIAN_POINT ( 'NONE',  ( 10.00000000000000000, -8.134922360106683570, 84.67002113262478247 ) ) ;
#2477 = FACE_OUTER_BOUND ( 'NONE', #20849, .T. ) ;
#2478 = CIRCLE ( 'NONE', #21187, 11.99999999999999822 ) ;
#2479 = ORIENTED_EDGE ( 'NONE', *, *, #12825, .F. ) ;
#2480 = DIRECTION ( 'NONE',  ( -1.000000000000000000, 0.000000000000000000, -0.000000000000000000 ) ) ;
#2481 = EDGE_LOOP ( 'NONE', ( #13688, #16346 ) ) ;
#2482 = EDGE_CURVE ( 'NONE', #9177, #4497, #7694, .T. ) ;
#2483 = VERTEX_POINT ( 'NONE', #10894 ) ;
#2484 = CARTESIAN_POINT ( 'NONE',  ( 0.000000000000000000, 45.60224695560681596, -80.47900393021679122 ) ) ;
#2485 = EDGE_CURVE ( 'NONE', #8212, #993, #8388, .T. ) ;
#2486 = DIRECTION ( 'NONE',  ( 1.000000000000000000, 0.000000000000000000, 0.000000000000000000 ) ) ;
#2487 = VERTEX_POINT ( 'NONE', #14431 ) ;
#2488 = EDGE_CURVE ( 'NONE', #18539, #8891, #4507, .T. ) ;
#2489 = ORIENTED_EDGE ( 'NONE', *, *, #8914, .F. ) ;
#2490 = ORIENTED_EDGE ( 'NONE', *, *, #4465, .F. ) ;
#2491 = ORIENTED_EDGE ( 'NONE', *, *, #10543, .T. ) ;
#2492 = CIRCLE ( 'NONE', #10954, 10.49999999999999822 ) ;
#2493 = DIRECTION ( 'NONE',  ( -0.000000000000000000, 0.000000000000000000, 1.000000000000000000 ) ) ;
#2494 = DIRECTION ( 'NONE',  ( -1.000000000000000000, 0.000000000000000000, 0.000000000000000000 ) ) ;
#2495 = ORIENTED_EDGE ( 'NONE', *, *, #9757, .T. ) ;
#2496 = CARTESIAN_POINT ( 'NONE',  ( 10.00000000000000000, 0.000000000000000000, 0.000000000000000000 ) ) ;
#2497 = FACE_OUTER_BOUND ( 'NONE', #10740, .T. ) ;
#2498 = FACE_OUTER_BOUND ( 'NONE', #21546, .T. ) ;
#2499 = LINE ( 'NONE', #7802, #7891 ) ;
#2500 = CARTESIAN_POINT ( 'NONE',  ( 0.000000000000000000, 21.98203405400955290, 17.64965094506551324 ) ) ;
#2501 = ORIENTED_EDGE ( 'NONE', *, *, #11447, .F. ) ;
#2502 = FACE_OUTER_BOUND ( 'NONE', #20642, .T. ) ;
#2503 = CARTESIAN_POINT ( 'NONE',  ( -10.00000000000000000, 0.000000000000000000, 0.000000000000000000 ) ) ;
#2504 = COLOUR_RGB ( '', 0.72549020, 0.75294118, 0.79215686) ;
#2505 = ADVANCED_BREP_SHAPE_REPRESENTATION ( '', ( #13597, #15567 ), #16627 ) ;
#2506 = CARTESIAN_POINT ( 'NONE',  ( 10.00000000000000000, -71.33759994382000968, 58.88447872958963814 ) ) ;
#2507 = VERTEX_POINT ( 'NONE', #14319 ) ;
#2508 = CARTESIAN_POINT ( 'NONE',  ( 1.400000000000000133, 0.000000000000000000, 0.000000000000000000 ) ) ;
#2509 = ORIENTED_EDGE ( 'NONE', *, *, #11386, .F. ) ;
#2510 = CARTESIAN_POINT ( 'NONE',  ( 0.000000000000000000, 0.000000000000000000, 0.000000000000000000 ) ) ;
#2511 = ORIENTED_EDGE ( 'NONE', *, *, #3520, .F. ) ;
#2512 = ORIENTED_EDGE ( 'NONE', *, *, #5125, .T. ) ;
#2513 = ORIENTED_EDGE ( 'NONE', *, *, #10171, .T. ) ;
#2514 = DIRECTION ( 'NONE',  ( -1.000000000000000000, 0.000000000000000000, 0.000000000000000000 ) ) ;
#2515 = ORIENTED_EDGE ( 'NONE', *, *, #20681, .T. ) ;
#2516 = DIRECTION ( 'NONE',  ( -1.000000000000000000, -0.000000000000000000, -0.000000000000000000 ) ) ;
#2517 = DIRECTION ( 'NONE',  ( 0.000000000000000000, 0.000000000000000000, -1.000000000000000000 ) ) ;
#2518 = DIRECTION ( 'NONE',  ( 0.000000000000000000, 0.000000000000000000, 1.000000000000000000 ) ) ;
#2519 = STYLED_ITEM ( 'NONE', ( #12189 ), #4298 ) ;
#2520 = DIRECTION ( 'NONE',  ( 0.000000000000000000, 0.000000000000000000, 1.000000000000000000 ) ) ;
#2521 = DIRECTION ( 'NONE',  ( -1.000000000000000000, 0.000000000000000000, -0.000000000000000000 ) ) ;
#2522 = DIRECTION ( 'NONE',  ( -1.000000000000000000, 0.000000000000000000, -0.000000000000000000 ) ) ;
#2523 = DIRECTION ( 'NONE',  ( 1.000000000000000000, 0.000000000000000000, 0.000000000000000000 ) ) ;
#2524 = CARTESIAN_POINT ( 'NONE',  ( 10.00000000000000000, -28.15804365424196121, -1.358152127006266197 ) ) ;
#2525 = DIRECTION ( 'NONE',  ( -1.000000000000000000, -0.000000000000000000, -0.000000000000000000 ) ) ;
#2526 = CARTESIAN_POINT ( 'NONE',  ( 5.000000000000002665, -86.77540292929691645, -14.62974526292806843 ) ) ;
#2527 = VERTEX_POINT ( 'NONE', #21064 ) ;
#2528 = EDGE_CURVE ( 'NONE', #19570, #6346, #5932, .T. ) ;
#2529 = ORIENTED_EDGE ( 'NONE', *, *, #12233, .F. ) ;
#2530 = ORIENTED_EDGE ( 'NONE', *, *, #19083, .T. ) ;
#2531 = ORIENTED_EDGE ( 'NONE', *, *, #3784, .F. ) ;
#2532 = EDGE_CURVE ( 'NONE', #13081, #1184, #18517, .T. ) ;
#2533 = ORIENTED_EDGE ( 'NONE', *, *, #17724, .T. ) ;
#2534 = DIRECTION ( 'NONE',  ( -1.000000000000000000, -0.000000000000000000, -0.000000000000000000 ) ) ;
#2535 = AXIS2_PLACEMENT_3D ( 'NONE', #10098, #10424, #15181 ) ;
#2536 = VERTEX_POINT ( 'NONE', #13533 ) ;
#2537 = DIRECTION ( 'NONE',  ( -1.000000000000000000, -0.000000000000000000, -0.000000000000000000 ) ) ;
#2538 = CARTESIAN_POINT ( 'NONE',  ( -7.600000000000002309, 0.000000000000000000, 0.000000000000000000 ) ) ;
#2539 = DIRECTION ( 'NONE',  ( 1.000000000000000000, 0.000000000000000000, -0.000000000000000000 ) ) ;
#2540 = DIRECTION ( 'NONE',  ( -1.000000000000000000, -0.000000000000000000, -0.000000000000000000 ) ) ;
#2541 = FACE_OUTER_BOUND ( 'NONE', #5263, .T. ) ;
#2542 = CYLINDRICAL_SURFACE ( 'NONE', #8325, 92.50100000000000477 ) ;
#2543 = DIRECTION ( 'NONE',  ( 0.000000000000000000, 0.3420201433256630508, 0.9396926207859105373 ) ) ;
#2544 = CARTESIAN_POINT ( 'NONE',  ( 0.000000000000000000, -51.10509369859380513, -77.10190917907254970 ) ) ;
#2545 = VECTOR ( 'NONE', #8853, 1000.000000000000000 ) ;
#2546 = ORIENTED_EDGE ( 'NONE', *, *, #18243, .F. ) ;
#2547 = CARTESIAN_POINT ( 'NONE',  ( 10.00000000000000000, 0.000000000000000000, 0.000000000000000000 ) ) ;
#2548 = VECTOR ( 'NONE', #9148, 1000.000000000000000 ) ;
#2549 = EDGE_CURVE ( 'NONE', #21817, #20730, #19790, .T. ) ;
#2550 = EDGE_CURVE ( 'NONE', #19310, #7770, #10222, .T. ) ;
#2551 = ADVANCED_FACE ( 'NONE', ( #11560 ), #20066, .T. ) ;
#2552 = DIRECTION ( 'NONE',  ( -1.000000000000000000, -0.000000000000000000, 0.000000000000000000 ) ) ;
#2553 = EDGE_CURVE ( 'NONE', #8941, #1477, #9190, .T. ) ;
#2554 = DIRECTION ( 'NONE',  ( -1.000000000000000000, -0.000000000000000000, -0.000000000000000000 ) ) ;
#2555 = VERTEX_POINT ( 'NONE', #11878 ) ;
#2556 = DIRECTION ( 'NONE',  ( 0.000000000000000000, 0.000000000000000000, 1.000000000000000000 ) ) ;
#2557 = ORIENTED_EDGE ( 'NONE', *, *, #5783, .F. ) ;
#2558 = ORIENTED_EDGE ( 'NONE', *, *, #12606, .T. ) ;
#2559 = DIRECTION ( 'NONE',  ( 1.000000000000000000, 0.000000000000000000, 0.000000000000000000 ) ) ;
#2560 = DIRECTION ( 'NONE',  ( 1.000000000000000000, 0.000000000000000000, 0.000000000000000000 ) ) ;
#2561 = AXIS2_PLACEMENT_3D ( 'NONE', #17012, #19004, #8609 ) ;
#2562 = VERTEX_POINT ( 'NONE', #20282 ) ;
#2563 = VERTEX_POINT ( 'NONE', #3050 ) ;
#2564 = FACE_OUTER_BOUND ( 'NONE', #13460, .T. ) ;
#2565 = CARTESIAN_POINT ( 'NONE',  ( 7.599999999999998757, 0.000000000000000000, -114.9007999999999896 ) ) ;
#2566 = EDGE_CURVE ( 'NONE', #20563, #13049, #1399, .T. ) ;
#2567 = CIRCLE ( 'NONE', #18812, 92.50100000000000477 ) ;
#2568 = AXIS2_PLACEMENT_3D ( 'NONE', #3633, #17344, #20865 ) ;
#2569 = CARTESIAN_POINT ( 'NONE',  ( 10.00000000000000000, -29.29369617358407041, -87.74003855418429509 ) ) ;
#2570 = FACE_OUTER_BOUND ( 'NONE', #14308, .T. ) ;
#2571 = CARTESIAN_POINT ( 'NONE',  ( 0.000000000000000000, 0.000000000000000000, 0.000000000000000000 ) ) ;
#2572 = DIRECTION ( 'NONE',  ( 0.000000000000000000, 0.000000000000000000, 1.000000000000000000 ) ) ;
#2573 = AXIS2_PLACEMENT_3D ( 'NONE', #18937, #7338, #15508 ) ;
#2574 = CARTESIAN_POINT ( 'NONE',  ( -140.0000507999999968, 0.000000000000000000, -5.000000000000000000 ) ) ;
#2575 = EDGE_CURVE ( 'NONE', #9950, #16436, #6385, .T. ) ;
#2576 = DIRECTION ( 'NONE',  ( 1.000000000000000000, 0.000000000000000000, 0.000000000000000000 ) ) ;
#2577 = CARTESIAN_POINT ( 'NONE',  ( 0.000000000000000000, 19.29292659244040564, -25.53004080487742300 ) ) ;
#2578 = ORIENTED_EDGE ( 'NONE', *, *, #2584, .F. ) ;
#2579 = DIRECTION ( 'NONE',  ( -1.000000000000000000, -0.000000000000000000, -0.000000000000000000 ) ) ;
#2580 = AXIS2_PLACEMENT_3D ( 'NONE', #8266, #9683, #6410 ) ;
#2581 = ORIENTED_EDGE ( 'NONE', *, *, #10962, .T. ) ;
#2582 = LINE ( 'NONE', #1049, #12961 ) ;
#2583 = VECTOR ( 'NONE', #1825, 1000.000000000000000 ) ;
#2584 = EDGE_CURVE ( 'NONE', #3353, #2487, #8028, .T. ) ;
#2585 = CARTESIAN_POINT ( 'NONE',  ( -90.00000000000000000, 0.000000000000000000, 0.000000000000000000 ) ) ;
#2586 = CARTESIAN_POINT ( 'NONE',  ( -90.00000000000000000, 1.284654492305574008E-14, 104.9000000000000341 ) ) ;
#2587 = ORIENTED_EDGE ( 'NONE', *, *, #16944, .T. ) ;
#2588 = CIRCLE ( 'NONE', #4012, 44.99999999999999289 ) ;
#2589 =( LENGTH_UNIT ( ) NAMED_UNIT ( * ) SI_UNIT ( .MILLI., .METRE. ) );
#2590 = AXIS2_PLACEMENT_3D ( 'NONE', #9742, #12952, #14726 ) ;
#2591 = ORIENTED_EDGE ( 'NONE', *, *, #13060, .F. ) ;
#2592 = ORIENTED_EDGE ( 'NONE', *, *, #14205, .T. ) ;
#2593 = ORIENTED_EDGE ( 'NONE', *, *, #18545, .F. ) ;
#2594 = DIRECTION ( 'NONE',  ( -1.000000000000000000, -0.000000000000000000, -0.000000000000000000 ) ) ;
#2595 = DIRECTION ( 'NONE',  ( 0.000000000000000000, -0.8660254037844328234, -0.5000000000000101030 ) ) ;
#2596 = VERTEX_POINT ( 'NONE', #21507 ) ;
#2597 = EDGE_CURVE ( 'NONE', #4038, #20275, #16853, .T. ) ;
#2598 = AXIS2_PLACEMENT_3D ( 'NONE', #10779, #20952, #17751 ) ;
#2599 = CARTESIAN_POINT ( 'NONE',  ( -7.395800000000001262, 0.000000000000000000, 0.000000000000000000 ) ) ;
#2600 = CARTESIAN_POINT ( 'NONE',  ( -7.599999999999999645, 114.9007999999999896, 0.000000000000000000 ) ) ;
#2601 = CARTESIAN_POINT ( 'NONE',  ( 7.999999999999979572, 0.000000000000000000, -115.1000000000000227 ) ) ;
#2602 = ADVANCED_FACE ( 'NONE', ( #18309 ), #5150, .F. ) ;
#2603 = DIRECTION ( 'NONE',  ( 0.000000000000000000, 0.000000000000000000, 1.000000000000000000 ) ) ;
#2604 = LINE ( 'NONE', #9226, #17915 ) ;
#2605 = AXIS2_PLACEMENT_3D ( 'NONE', #6887, #1575, #5000 ) ;
#2606 = EDGE_CURVE ( 'NONE', #15305, #16104, #18194, .T. ) ;
#2607 = VERTEX_POINT ( 'NONE', #16736 ) ;
#2608 = AXIS2_PLACEMENT_3D ( 'NONE', #21498, #9881, #19500 ) ;
#2609 = EDGE_CURVE ( 'NONE', #18821, #2865, #6407, .T. ) ;
#2610 = CYLINDRICAL_SURFACE ( 'NONE', #21852, 88.00000000000000000 ) ;
#2611 = DIRECTION ( 'NONE',  ( -1.000000000000000000, -0.000000000000000000, -0.000000000000000000 ) ) ;
#2612 = CARTESIAN_POINT ( 'NONE',  ( 10.00000000000000000, -27.87320266523616752, 88.20158487341750231 ) ) ;
#2613 = VERTEX_POINT ( 'NONE', #11669 ) ;
#2614 = AXIS2_PLACEMENT_3D ( 'NONE', #21710, #6595, #20064 ) ;
#2615 = ADVANCED_FACE ( 'NONE', ( #3485 ), #19834, .F. ) ;
#2616 = DIRECTION ( 'NONE',  ( 1.000000000000000000, 0.000000000000000000, 0.000000000000000000 ) ) ;
#2617 = EDGE_LOOP ( 'NONE', ( #18680, #16035, #2578, #11756 ) ) ;
#2618 = DIRECTION ( 'NONE',  ( 0.000000000000000000, 0.000000000000000000, 1.000000000000000000 ) ) ;
#2619 = VERTEX_POINT ( 'NONE', #4700 ) ;
#2620 = AXIS2_PLACEMENT_3D ( 'NONE', #833, #7578, #5927 ) ;
#2621 = ORIENTED_EDGE ( 'NONE', *, *, #17837, .T. ) ;
#2622 = ORIENTED_EDGE ( 'NONE', *, *, #13020, .T. ) ;
#2623 = CYLINDRICAL_SURFACE ( 'NONE', #7273, 45.00000000000000000 ) ;
#2624 = CIRCLE ( 'NONE', #18867, 88.00000000000000000 ) ;
#2625 = VERTEX_POINT ( 'NONE', #1607 ) ;
#2626 = LINE ( 'NONE', #2743, #1012 ) ;
#2627 = CARTESIAN_POINT ( 'NONE',  ( 10.00000000000000000, 47.19205848891765243, 74.27590198428138990 ) ) ;
#2628 = DIRECTION ( 'NONE',  ( -1.000000000000000000, -0.000000000000000000, -0.000000000000000000 ) ) ;
#2629 = DIRECTION ( 'NONE',  ( 0.000000000000000000, 0.000000000000000000, 1.000000000000000000 ) ) ;
#2630 = AXIS2_PLACEMENT_3D ( 'NONE', #3431, #21475, #11824 ) ;
#2631 = CARTESIAN_POINT ( 'NONE',  ( 10.00000000000000000, -19.07277123396555041, 19.80970465344741882 ) ) ;
#2632 = CIRCLE ( 'NONE', #1579, 11.99999999999999822 ) ;
#2633 = DIRECTION ( 'NONE',  ( 0.000000000000000000, -0.9271838545667832054, -0.3746065934159225619 ) ) ;
#2634 = VECTOR ( 'NONE', #14339, 1000.000000000000000 ) ;
#2635 = FACE_OUTER_BOUND ( 'NONE', #18479, .T. ) ;
#2636 = DIRECTION ( 'NONE',  ( 1.000000000000000000, 0.000000000000000000, 0.000000000000000000 ) ) ;
#2637 = CIRCLE ( 'NONE', #20283, 88.00000000000000000 ) ;
#2638 = TOROIDAL_SURFACE ( 'NONE', #15701, 118.9000000000000199, 1.100000000000015854 ) ;
#2639 = LINE ( 'NONE', #2526, #926 ) ;
#2640 = ORIENTED_EDGE ( 'NONE', *, *, #20917, .T. ) ;
#2641 = ORIENTED_EDGE ( 'NONE', *, *, #12685, .F. ) ;
#2642 = ORIENTED_EDGE ( 'NONE', *, *, #14904, .T. ) ;
#2643 = ORIENTED_EDGE ( 'NONE', *, *, #3209, .T. ) ;
#2644 = CIRCLE ( 'NONE', #15001, 12.00000000000000000 ) ;
#2645 = AXIS2_PLACEMENT_3D ( 'NONE', #16197, #14535, #10778 ) ;
#2646 = VERTEX_POINT ( 'NONE', #8349 ) ;
#2647 = AXIS2_PLACEMENT_3D ( 'NONE', #16940, #5333, #8635 ) ;
#2648 = DIRECTION ( 'NONE',  ( -1.000000000000000000, 0.000000000000000000, -0.000000000000000000 ) ) ;
#2649 = ORIENTED_EDGE ( 'NONE', *, *, #6913, .F. ) ;
#2650 = CARTESIAN_POINT ( 'NONE',  ( 10.00000000000000000, 0.000000000000000000, 0.000000000000000000 ) ) ;
#2651 = DIRECTION ( 'NONE',  ( -1.000000000000000000, -0.000000000000000000, -0.000000000000000000 ) ) ;
#2652 = AXIS2_PLACEMENT_3D ( 'NONE', #9795, #1422, #13223 ) ;
#2653 = FACE_OUTER_BOUND ( 'NONE', #9378, .T. ) ;
#2654 = DIRECTION ( 'NONE',  ( 0.000000000000000000, 0.000000000000000000, 1.000000000000000000 ) ) ;
#2655 = DIRECTION ( 'NONE',  ( -1.000000000000000000, -0.000000000000000000, -0.000000000000000000 ) ) ;
#2656 = ADVANCED_FACE ( 'NONE', ( #15078 ), #21825, .F. ) ;
#2657 = CARTESIAN_POINT ( 'NONE',  ( 0.000000000000000000, 0.000000000000000000, 9.999999999999998224 ) ) ;
#2658 = LINE ( 'NONE', #12811, #13964 ) ;
#2659 = CARTESIAN_POINT ( 'NONE',  ( -8.000000000000007105, 0.000000000000000000, 0.000000000000000000 ) ) ;
#2660 = CARTESIAN_POINT ( 'NONE',  ( 0.000000000000000000, 0.000000000000000000, 0.000000000000000000 ) ) ;
#2661 = AXIS2_PLACEMENT_3D ( 'NONE', #4605, #21399, #6277 ) ;
#2662 = VERTEX_POINT ( 'NONE', #5032 ) ;
#2663 = AXIS2_PLACEMENT_3D ( 'NONE', #5561, #261, #17169 ) ;
#2664 = PRODUCT_RELATED_PRODUCT_CATEGORY ( 'part', '', ( #8086 ) ) ;
#2665 = AXIS2_PLACEMENT_3D ( 'NONE', #11325, #16849, #3369 ) ;
#2666 = CARTESIAN_POINT ( 'NONE',  ( 0.000000000000000000, 30.61448696004452685, 9.314139153634330981 ) ) ;
#2667 = AXIS2_PLACEMENT_3D ( 'NONE', #9173, #17369, #5659 ) ;
#2668 = VERTEX_POINT ( 'NONE', #15190 ) ;
#2669 = DIRECTION ( 'NONE',  ( 0.000000000000000000, 0.000000000000000000, 1.000000000000000000 ) ) ;
#2670 = DIRECTION ( 'NONE',  ( 0.000000000000000000, 0.000000000000000000, 1.000000000000000000 ) ) ;
#2671 = ORIENTED_EDGE ( 'NONE', *, *, #14760, .T. ) ;
#2672 = CARTESIAN_POINT ( 'NONE',  ( 10.00000000000000000, 81.55207211302045778, 24.17537951050201883 ) ) ;
#2673 = ORIENTED_EDGE ( 'NONE', *, *, #13687, .F. ) ;
#2674 = VERTEX_POINT ( 'NONE', #11768 ) ;
#2675 = CIRCLE ( 'NONE', #14318, 11.99999999999999822 ) ;
#2676 = DIRECTION ( 'NONE',  ( 0.000000000000000000, 0.000000000000000000, 1.000000000000000000 ) ) ;
#2677 = CARTESIAN_POINT ( 'NONE',  ( 10.00000000000000000, -14.53731623274912366, -23.34226719384920656 ) ) ;
#2678 = ORIENTED_EDGE ( 'NONE', *, *, #14481, .T. ) ;
#2679 = VECTOR ( 'NONE', #19900, 1000.000000000000000 ) ;
#2680 = EDGE_LOOP ( 'NONE', ( #8458, #4593, #12132, #11621 ) ) ;
#2681 = DIRECTION ( 'NONE',  ( 0.000000000000000000, 0.000000000000000000, 1.000000000000000000 ) ) ;
#2682 = DIRECTION ( 'NONE',  ( 0.000000000000000000, 0.000000000000000000, -1.000000000000000000 ) ) ;
#2683 = CIRCLE ( 'NONE', #21337, 11.99999999999999822 ) ;
#2684 = CARTESIAN_POINT ( 'NONE',  ( 10.00000000000000000, 57.47876254627226444, -62.70072803846332476 ) ) ;
#2685 = DIRECTION ( 'NONE',  ( 1.000000000000000000, 0.000000000000000000, 0.000000000000000000 ) ) ;
#2686 = ADVANCED_FACE ( 'NONE', ( #12089 ), #13858, .F. ) ;
#2687 = CARTESIAN_POINT ( 'NONE',  ( 10.00000000000000000, 0.000000000000000000, 0.000000000000000000 ) ) ;
#2688 = CARTESIAN_POINT ( 'NONE',  ( 10.00000000000000000, -21.65267340503189430, -89.93106657554454841 ) ) ;
#2689 = DIRECTION ( 'NONE',  ( 0.000000000000000000, 0.6946583704589983643, -0.7193398003386500816 ) ) ;
#2690 = DIRECTION ( 'NONE',  ( -1.000000000000000000, 0.000000000000000000, 0.000000000000000000 ) ) ;
#2691 = DIRECTION ( 'NONE',  ( 0.000000000000000000, 0.000000000000000000, 1.000000000000000000 ) ) ;
#2692 = ORIENTED_EDGE ( 'NONE', *, *, #7676, .F. ) ;
#2693 = CARTESIAN_POINT ( 'NONE',  ( 10.00000000000000000, 78.83848282823974785, -48.38314403117421847 ) ) ;
#2694 = ORIENTED_EDGE ( 'NONE', *, *, #321, .F. ) ;
#2695 = CIRCLE ( 'NONE', #18250, 88.00000000000000000 ) ;
#2696 = CIRCLE ( 'NONE', #12228, 44.99999999999998579 ) ;
#2697 = DIRECTION ( 'NONE',  ( -1.000000000000000000, -0.000000000000000000, 0.000000000000000000 ) ) ;
#2698 = ADVANCED_FACE ( 'NONE', ( #7026 ), #12313, .F. ) ;
#2699 = CARTESIAN_POINT ( 'NONE',  ( 0.000000000000000000, 23.37352460145283928, 21.85585385440887762 ) ) ;
#2700 = CARTESIAN_POINT ( 'NONE',  ( -90.00000000000000000, 0.000000000000000000, 0.000000000000000000 ) ) ;
#2701 = ORIENTED_EDGE ( 'NONE', *, *, #7045, .F. ) ;
#2702 = EDGE_CURVE ( 'NONE', #21564, #10277, #8437, .T. ) ;
#2703 = ORIENTED_EDGE ( 'NONE', *, *, #2335, .F. ) ;
#2704 = ORIENTED_EDGE ( 'NONE', *, *, #15351, .F. ) ;
#2705 = ORIENTED_EDGE ( 'NONE', *, *, #3213, .T. ) ;
#2706 = LINE ( 'NONE', #4809, #16007 ) ;
#2707 = DIRECTION ( 'NONE',  ( 0.000000000000000000, 0.9848077530122084644, -0.1736481776669273336 ) ) ;
#2708 = ORIENTED_EDGE ( 'NONE', *, *, #19121, .T. ) ;
#2709 = CIRCLE ( 'NONE', #21764, 88.00000000000000000 ) ;
#2710 = EDGE_CURVE ( 'NONE', #12003, #5459, #14415, .T. ) ;
#2711 = CARTESIAN_POINT ( 'NONE',  ( 10.00000000000000000, -25.17124263951000529, -12.69364185792245081 ) ) ;
#2712 = CARTESIAN_POINT ( 'NONE',  ( 10.00000000000000000, 31.75612719289746266, -3.943144139962236228 ) ) ;
#2713 = ADVANCED_FACE ( 'NONE', ( #6919 ), #19057, .F. ) ;
#2714 = VECTOR ( 'NONE', #16423, 1000.000000000000000 ) ;
#2715 = DIRECTION ( 'NONE',  ( -1.000000000000000000, 0.000000000000000000, -0.000000000000000000 ) ) ;
#2716 = EDGE_CURVE ( 'NONE', #11894, #7808, #13356, .T. ) ;
#2717 = DIRECTION ( 'NONE',  ( -1.000000000000000000, 0.000000000000000000, 0.000000000000000000 ) ) ;
#2718 = VECTOR ( 'NONE', #866, 1000.000000000000000 ) ;
#2719 = DIRECTION ( 'NONE',  ( 0.000000000000000000, 0.000000000000000000, -1.000000000000000000 ) ) ;
#2720 = EDGE_CURVE ( 'NONE', #21761, #8420, #5256, .T. ) ;
#2721 = ORIENTED_EDGE ( 'NONE', *, *, #5400, .F. ) ;
#2722 = CARTESIAN_POINT ( 'NONE',  ( -7.440711023145607506, 0.000000000000000000, 0.000000000000000000 ) ) ;
#2723 = LINE ( 'NONE', #4271, #19244 ) ;
#2724 = EDGE_LOOP ( 'NONE', ( #20486, #7003, #4348, #21102 ) ) ;
#2725 = DIRECTION ( 'NONE',  ( 1.000000000000000000, 0.000000000000000000, 0.000000000000000000 ) ) ;
#2726 = ADVANCED_FACE ( 'NONE', ( #11988 ), #13643, .F. ) ;
#2727 = ORIENTED_EDGE ( 'NONE', *, *, #13366, .T. ) ;
#2728 = VECTOR ( 'NONE', #9045, 1000.000000000000000 ) ;
#2729 = DIRECTION ( 'NONE',  ( 1.000000000000000000, 0.000000000000000000, 0.000000000000000000 ) ) ;
#2730 = CIRCLE ( 'NONE', #3444, 92.50100000000000477 ) ;
#2731 = DIRECTION ( 'NONE',  ( 1.000000000000000000, 0.000000000000000000, 0.000000000000000000 ) ) ;
#2732 = ADVANCED_FACE ( 'NONE', ( #15292 ), #5578, .F. ) ;
#2733 = AXIS2_PLACEMENT_3D ( 'NONE', #7058, #20200, #15437 ) ;
#2734 = ORIENTED_EDGE ( 'NONE', *, *, #21329, .T. ) ;
#2735 = DIRECTION ( 'NONE',  ( 1.000000000000000000, 0.000000000000000000, 0.000000000000000000 ) ) ;
#2736 = EDGE_CURVE ( 'NONE', #18369, #7224, #4018, .T. ) ;
#2737 = ORIENTED_EDGE ( 'NONE', *, *, #7207, .T. ) ;
#2738 = EDGE_LOOP ( 'NONE', ( #17858, #2737, #11761, #13895 ) ) ;
#2739 = ORIENTED_EDGE ( 'NONE', *, *, #13154, .T. ) ;
#2740 = CARTESIAN_POINT ( 'NONE',  ( 10.00000000000000000, 9.646732466566502850, -84.51112348751837544 ) ) ;
#2741 = EDGE_CURVE ( 'NONE', #19412, #16260, #18841, .T. ) ;
#2742 = VERTEX_POINT ( 'NONE', #8673 ) ;
#2743 = CARTESIAN_POINT ( 'NONE',  ( 5.000000000000000000, -83.48638250753248258, 27.82128566055087049 ) ) ;
#2744 = LINE ( 'NONE', #20975, #7241 ) ;
#2745 = CARTESIAN_POINT ( 'NONE',  ( 10.00000000000000000, 0.000000000000000000, 0.000000000000000000 ) ) ;
#2746 = DIRECTION ( 'NONE',  ( -1.000000000000000000, 0.000000000000000000, 0.000000000000000000 ) ) ;
#2747 = AXIS2_PLACEMENT_3D ( 'NONE', #6989, #3983, #8950 ) ;
#2748 = EDGE_CURVE ( 'NONE', #21192, #2262, #3226, .T. ) ;
#2749 = AXIS2_PLACEMENT_3D ( 'NONE', #16510, #15060, #21692 ) ;
#2750 = LINE ( 'NONE', #2631, #4837 ) ;
#2751 = CARTESIAN_POINT ( 'NONE',  ( 10.00000000000000000, -80.18694381077126820, 28.37681241246628616 ) ) ;
#2752 = AXIS2_PLACEMENT_3D ( 'NONE', #5492, #406, #5380 ) ;
#2753 = AXIS2_PLACEMENT_3D ( 'NONE', #6359, #15164, #14732 ) ;
#2755 = EDGE_CURVE ( 'NONE', #21410, #5809, #10645, .T. ) ;
#2754 = CARTESIAN_POINT ( 'NONE',  ( 10.00000000000000000, -32.56745702629687855, -78.57830605990686479 ) ) ;
#2756 = DIRECTION ( 'NONE',  ( 1.000000000000000000, 0.000000000000000000, 0.000000000000000000 ) ) ;
#2757 = DIRECTION ( 'NONE',  ( 1.000000000000000000, 0.000000000000000000, 0.000000000000000000 ) ) ;
#2758 =( REPRESENTATION_RELATIONSHIP ('NONE','NONE', #2177, #10365 ) REPRESENTATION_RELATIONSHIP_WITH_TRANSFORMATION ( #6562 )SHAPE_REPRESENTATION_RELATIONSHIP( ) );
#2759 = ORIENTED_EDGE ( 'NONE', *, *, #4928, .T. ) ;
#2760 = ORIENTED_EDGE ( 'NONE', *, *, #7713, .T. ) ;
#2761 = EDGE_CURVE ( 'NONE', #12158, #11505, #388, .T. ) ;
#2762 = ORIENTED_EDGE ( 'NONE', *, *, #2720, .T. ) ;
#2763 = CIRCLE ( 'NONE', #14769, 92.50100000000000477 ) ;
#2764 = EDGE_LOOP ( 'NONE', ( #4176, #1480, #20463, #16420 ) ) ;
#2765 = AXIS2_PLACEMENT_3D ( 'NONE', #7765, #2552, #20803 ) ;
#2766 = AXIS2_PLACEMENT_3D ( 'NONE', #19687, #9729, #4772 ) ;
#2767 = AXIS2_PLACEMENT_3D ( 'NONE', #579, #11171, #6099 ) ;
#2768 = EDGE_CURVE ( 'NONE', #4275, #19773, #7237, .T. ) ;
#2769 = VERTEX_POINT ( 'NONE', #12204 ) ;
#2770 = FACE_OUTER_BOUND ( 'NONE', #850, .T. ) ;
#2771 = EDGE_LOOP ( 'NONE', ( #19821, #15, #5275, #8334 ) ) ;
#2772 = CARTESIAN_POINT ( 'NONE',  ( -1.500000000000000000, 15.00000000000000000, 0.000000000000000000 ) ) ;
#2773 = DIRECTION ( 'NONE',  ( 1.000000000000000000, 0.000000000000000000, 0.000000000000000000 ) ) ;
#2774 = CARTESIAN_POINT ( 'NONE',  ( 10.00000000000000000, 27.26034713664097353, -7.182859710736244629 ) ) ;
#2775 = FACE_OUTER_BOUND ( 'NONE', #1912, .T. ) ;
#2776 = CARTESIAN_POINT ( 'NONE',  ( -90.00000000000000000, 6.873330160214519262E-16, 5.612499999999999822 ) ) ;
#2777 = DIRECTION ( 'NONE',  ( 1.000000000000000000, 0.000000000000000000, 0.000000000000000000 ) ) ;
#2778 = LINE ( 'NONE', #9274, #8020 ) ;
#2779 = DIRECTION ( 'NONE',  ( 0.000000000000000000, 0.000000000000000000, 1.000000000000000000 ) ) ;
#2780 = AXIS2_PLACEMENT_3D ( 'NONE', #15669, #6854, #3747 ) ;
#2781 = AXIS2_PLACEMENT_3D ( 'NONE', #2403, #10587, #15773 ) ;
#2782 = VECTOR ( 'NONE', #15658, 1000.000000000000000 ) ;
#2783 = AXIS2_PLACEMENT_3D ( 'NONE', #3915, #8564, #3697 ) ;
#2784 = ORIENTED_EDGE ( 'NONE', *, *, #18493, .F. ) ;
#2785 = AXIS2_PLACEMENT_3D ( 'NONE', #17244, #8840, #13472 ) ;
#2786 = CARTESIAN_POINT ( 'NONE',  ( 10.00000000000000000, 0.000000000000000000, 0.000000000000000000 ) ) ;
#2787 = EDGE_LOOP ( 'NONE', ( #17301, #12451, #2092, #4171 ) ) ;
#2788 = EDGE_CURVE ( 'NONE', #12003, #3216, #20524, .T. ) ;
#2789 = DIRECTION ( 'NONE',  ( -1.000000000000000000, 0.000000000000000000, 0.000000000000000000 ) ) ;
#2790 = DIRECTION ( 'NONE',  ( 0.000000000000000000, 0.6427876096865403621, -0.7660444431189772363 ) ) ;
#2791 = EDGE_LOOP ( 'NONE', ( #1507, #989, #4089, #3085, #18940 ) ) ;
#2792 = FACE_OUTER_BOUND ( 'NONE', #3643, .T. ) ;
#2793 = ORIENTED_EDGE ( 'NONE', *, *, #16804, .F. ) ;
#2794 = ORIENTED_EDGE ( 'NONE', *, *, #21494, .F. ) ;
#2795 = SHAPE_DEFINITION_REPRESENTATION ( #4917, #16445 ) ;
#2796 = VECTOR ( 'NONE', #21843, 1000.000000000000000 ) ;
#2797 = CARTESIAN_POINT ( 'NONE',  ( 5.000000000000002665, 0.6609040254623512745, -87.99751818016873983 ) ) ;
#2798 = ORIENTED_EDGE ( 'NONE', *, *, #16944, .F. ) ;
#2799 = CIRCLE ( 'NONE', #663, 11.99999999999999645 ) ;
#2800 = ORIENTED_EDGE ( 'NONE', *, *, #1906, .T. ) ;
#2801 = DIRECTION ( 'NONE',  ( -1.000000000000000000, -0.000000000000000000, -0.000000000000000000 ) ) ;
#2802 = STYLED_ITEM ( 'NONE', ( #15197 ), #20649 ) ;
#2803 = AXIS2_PLACEMENT_3D ( 'NONE', #16773, #15215, #3408 ) ;
#2804 = DIRECTION ( 'NONE',  ( -1.000000000000000000, -0.000000000000000000, -0.000000000000000000 ) ) ;
#2805 = CARTESIAN_POINT ( 'NONE',  ( 10.00000000000000000, 0.000000000000000000, 0.000000000000000000 ) ) ;
#2806 = DIRECTION ( 'NONE',  ( -1.000000000000000000, 0.000000000000000000, 0.000000000000000000 ) ) ;
#2807 = CYLINDRICAL_SURFACE ( 'NONE', #6872, 11.99999999999999645 ) ;
#2808 = FACE_OUTER_BOUND ( 'NONE', #17080, .T. ) ;
#2809 = CARTESIAN_POINT ( 'NONE',  ( 10.00000000000000000, -24.73395913766471921, 12.01774797440568854 ) ) ;
#2810 = DIRECTION ( 'NONE',  ( -0.000000000000000000, -0.000000000000000000, 1.000000000000000000 ) ) ;
#2811 = ORIENTED_EDGE ( 'NONE', *, *, #19488, .F. ) ;
#2812 = CARTESIAN_POINT ( 'NONE',  ( 10.00000000000000000, 0.000000000000000000, 0.000000000000000000 ) ) ;
#2813 = AXIS2_PLACEMENT_3D ( 'NONE', #19697, #4667, #11404 ) ;
#2814 = ORIENTED_EDGE ( 'NONE', *, *, #18781, .F. ) ;
#2815 = CIRCLE ( 'NONE', #15155, 92.50100000000000477 ) ;
#2816 = AXIS2_PLACEMENT_3D ( 'NONE', #9896, #5153, #7028 ) ;
#2817 = DIRECTION ( 'NONE',  ( 0.000000000000000000, 0.000000000000000000, 1.000000000000000000 ) ) ;
#2818 = EDGE_CURVE ( 'NONE', #18794, #17904, #17298, .T. ) ;
#2819 = CARTESIAN_POINT ( 'NONE',  ( 0.000000000000000000, 0.000000000000000000, 3.000000000000000000 ) ) ;
#2820 = ORIENTED_EDGE ( 'NONE', *, *, #17323, .T. ) ;
#2821 = ORIENTED_EDGE ( 'NONE', *, *, #19984, .T. ) ;
#2822 = EDGE_LOOP ( 'NONE', ( #5751, #7159, #11396, #1890 ) ) ;
#2823 = ORIENTED_EDGE ( 'NONE', *, *, #7215, .T. ) ;
#2824 = DIRECTION ( 'NONE',  ( 1.000000000000000000, 0.000000000000000000, 0.000000000000000000 ) ) ;
#2825 = EDGE_CURVE ( 'NONE', #12372, #9325, #411, .T. ) ;
#2826 = EDGE_LOOP ( 'NONE', ( #10289, #16219, #3929, #4299 ) ) ;
#2827 = CARTESIAN_POINT ( 'NONE',  ( 0.000000000000000000, 77.39385041987151226, -35.28996114464630551 ) ) ;
#2828 = LINE ( 'NONE', #16295, #18592 ) ;
#2829 = LINE ( 'NONE', #17646, #17125 ) ;
#2830 = CIRCLE ( 'NONE', #5653, 88.00000000000000000 ) ;
#2831 = DIRECTION ( 'NONE',  ( -1.000000000000000000, -0.000000000000000000, 0.000000000000000000 ) ) ;
#2832 = DIRECTION ( 'NONE',  ( 1.000000000000000000, 0.000000000000000000, 0.000000000000000000 ) ) ;
#2833 = ADVANCED_FACE ( 'NONE', ( #9303 ), #7454, .T. ) ;
#2834 = ORIENTED_EDGE ( 'NONE', *, *, #13831, .F. ) ;
#2835 = DIRECTION ( 'NONE',  ( 1.000000000000000000, 0.000000000000000000, 0.000000000000000000 ) ) ;
#2836 = CARTESIAN_POINT ( 'NONE',  ( 10.00000000000000000, 92.32475887865433606, -5.707354816229567973 ) ) ;
#2837 = EDGE_LOOP ( 'NONE', ( #17354, #17175, #16867, #1234 ) ) ;
#2838 = CARTESIAN_POINT ( 'NONE',  ( 10.00000000000000000, 9.992993448021589842, 26.36019881529889020 ) ) ;
#2839 = EDGE_LOOP ( 'NONE', ( #5345, #2376, #6902, #12220 ) ) ;
#2840 = EDGE_CURVE ( 'NONE', #5619, #17311, #14287, .T. ) ;
#2841 = DIRECTION ( 'NONE',  ( 1.000000000000000000, 0.000000000000000000, 0.000000000000000000 ) ) ;
#2842 = ADVANCED_FACE ( 'NONE', ( #4245 ), #8041, .T. ) ;
#2843 = EDGE_CURVE ( 'NONE', #4620, #2079, #7886, .T. ) ;
#2844 = CIRCLE ( 'NONE', #4976, 5.453125000000000000 ) ;
#2845 = CARTESIAN_POINT ( 'NONE',  ( 0.000000000000000000, -47.19205848891713373, -74.27590198428171675 ) ) ;
#2846 = ORIENTED_EDGE ( 'NONE', *, *, #17293, .F. ) ;
#2847 = CARTESIAN_POINT ( 'NONE',  ( 0.000000000000000000, 0.000000000000000000, 0.000000000000000000 ) ) ;
#2848 = EDGE_CURVE ( 'NONE', #17141, #10612, #19481, .T. ) ;
#2849 = VERTEX_POINT ( 'NONE', #14619 ) ;
#2850 = VERTEX_POINT ( 'NONE', #19269 ) ;
#2851 = DIRECTION ( 'NONE',  ( 1.000000000000000000, -0.000000000000000000, -0.000000000000000000 ) ) ;
#2852 = VERTEX_POINT ( 'NONE', #21364 ) ;
#2853 = CYLINDRICAL_SURFACE ( 'NONE', #19735, 11.99999999999999822 ) ;
#2854 = DIRECTION ( 'NONE',  ( -1.000000000000000000, -0.000000000000000000, -0.000000000000000000 ) ) ;
#2855 = CARTESIAN_POINT ( 'NONE',  ( 0.000000000000000000, 0.000000000000000000, 0.000000000000000000 ) ) ;
#2856 = DIRECTION ( 'NONE',  ( 0.000000000000000000, 0.1391731009600657432, -0.9902680687415702510 ) ) ;
#2857 = ADVANCED_FACE ( 'NONE', ( #5905 ), #6026, .F. ) ;
#2858 = CARTESIAN_POINT ( 'NONE',  ( 10.00000000000000000, -11.59241532900687233, 87.23311244498734141 ) ) ;
#2859 = CARTESIAN_POINT ( 'NONE',  ( 10.00000000000000000, 19.29292659244040564, -25.53004080487741945 ) ) ;
#2860 = DIRECTION ( 'NONE',  ( -1.000000000000000000, 0.000000000000000000, -0.000000000000000000 ) ) ;
#2861 = EDGE_CURVE ( 'NONE', #5782, #5530, #20315, .T. ) ;
#2862 = CARTESIAN_POINT ( 'NONE',  ( 0.000000000000000000, 89.12061559554332746, 24.77803214283573396 ) ) ;
#2863 = DIRECTION ( 'NONE',  ( 1.000000000000000000, 0.000000000000000000, 0.000000000000000000 ) ) ;
#2864 = ORIENTED_EDGE ( 'NONE', *, *, #8900, .T. ) ;
#2865 = VERTEX_POINT ( 'NONE', #4134 ) ;
#2866 = ORIENTED_EDGE ( 'NONE', *, *, #7314, .F. ) ;
#2867 = EDGE_CURVE ( 'NONE', #18968, #8553, #17487, .T. ) ;
#2868 = ORIENTED_EDGE ( 'NONE', *, *, #4512, .F. ) ;
#2869 = VERTEX_POINT ( 'NONE', #4345 ) ;
#2870 = CARTESIAN_POINT ( 'NONE',  ( 10.00000000000000000, -27.26034713664092379, -7.182859710736426706 ) ) ;
#2871 = VERTEX_POINT ( 'NONE', #12632 ) ;
#2872 = DIRECTION ( 'NONE',  ( -1.000000000000000000, -0.000000000000000000, -0.000000000000000000 ) ) ;
#2873 = CARTESIAN_POINT ( 'NONE',  ( 0.000000000000000000, 7.409634587003093742, 27.19958299168160565 ) ) ;
#2874 = EDGE_CURVE ( 'NONE', #8708, #11578, #19382, .T. ) ;
#2875 = CARTESIAN_POINT ( 'NONE',  ( 0.000000000000000000, 0.000000000000000000, 0.000000000000000000 ) ) ;
#2876 = CARTESIAN_POINT ( 'NONE',  ( 0.000000000000000000, -8.134922360106683570, 84.67002113262478247 ) ) ;
#2877 = CARTESIAN_POINT ( 'NONE',  ( 10.00000000000000000, 81.97107881582195432, 22.71412948308594437 ) ) ;
#2878 = EDGE_CURVE ( 'NONE', #2527, #15117, #9102, .T. ) ;
#2879 = DIRECTION ( 'NONE',  ( -1.000000000000000000, -0.000000000000000000, -0.000000000000000000 ) ) ;
#2880 = CARTESIAN_POINT ( 'NONE',  ( 0.000000000000000000, 3.974475837766159980, -92.41557521768187655 ) ) ;
#2881 = MECHANICAL_DESIGN_GEOMETRIC_PRESENTATION_REPRESENTATION (  '', ( #21577 ), #20179 ) ;
#2882 = EDGE_CURVE ( 'NONE', #10824, #8047, #7247, .T. ) ;
#2883 = VERTEX_POINT ( 'NONE', #9201 ) ;
#2884 = EDGE_CURVE ( 'NONE', #1840, #19484, #17136, .T. ) ;
#2885 = DIRECTION ( 'NONE',  ( 0.000000000000000000, 0.000000000000000000, 1.000000000000000000 ) ) ;
#2886 = ORIENTED_EDGE ( 'NONE', *, *, #8646, .T. ) ;
#2887 = ORIENTED_EDGE ( 'NONE', *, *, #3656, .F. ) ;
#2888 = AXIS2_PLACEMENT_3D ( 'NONE', #4841, #11582, #3287 ) ;
#2889 = DIRECTION ( 'NONE',  ( -1.000000000000000000, 0.000000000000000000, -0.000000000000000000 ) ) ;
#2890 = DIRECTION ( 'NONE',  ( -1.000000000000000000, -0.000000000000000000, -0.000000000000000000 ) ) ;
#2891 = ORIENTED_EDGE ( 'NONE', *, *, #5684, .F. ) ;
#2892 = DIRECTION ( 'NONE',  ( -1.000000000000000000, 0.000000000000000000, 0.000000000000000000 ) ) ;
#2893 = ORIENTED_EDGE ( 'NONE', *, *, #6691, .F. ) ;
#2894 = ORIENTED_EDGE ( 'NONE', *, *, #10989, .F. ) ;
#2895 = PRODUCT_CONTEXT ( 'NONE', #11362, 'mechanical' ) ;
#2896 = CARTESIAN_POINT ( 'NONE',  ( 0.000000000000000000, 15.32665449651924661, 91.22241316115426457 ) ) ;
#2897 = ORIENTED_EDGE ( 'NONE', *, *, #18483, .T. ) ;
#2898 = EDGE_LOOP ( 'NONE', ( #8789, #10979, #4690, #11709 ) ) ;
#2899 = DIRECTION ( 'NONE',  ( 0.000000000000000000, 0.000000000000000000, 1.000000000000000000 ) ) ;
#2900 = CYLINDRICAL_SURFACE ( 'NONE', #6693, 92.50100000000000477 ) ;
#2901 = AXIS2_PLACEMENT_3D ( 'NONE', #1459, #10290, #17036 ) ;
#2902 = DIRECTION ( 'NONE',  ( -1.000000000000000000, 0.000000000000000000, 0.000000000000000000 ) ) ;
#2903 = CARTESIAN_POINT ( 'NONE',  ( 10.00000000000000000, 68.36541360927188293, 50.60987712331726840 ) ) ;
#2904 = DIRECTION ( 'NONE',  ( 0.000000000000000000, 0.8290375725550428454, -0.5591929034707450175 ) ) ;
#2905 = DIRECTION ( 'NONE',  ( 0.000000000000000000, 0.000000000000000000, 1.000000000000000000 ) ) ;
#2906 = DIRECTION ( 'NONE',  ( 0.000000000000000000, 0.000000000000000000, 1.000000000000000000 ) ) ;
#2907 = DIRECTION ( 'NONE',  ( -1.000000000000000000, -0.000000000000000000, -0.000000000000000000 ) ) ;
#2908 = LINE ( 'NONE', #3024, #8757 ) ;
#2909 = VECTOR ( 'NONE', #12081, 1000.000000000000000 ) ;
#2910 = VERTEX_POINT ( 'NONE', #5794 ) ;
#2911 = AXIS2_PLACEMENT_3D ( 'NONE', #87, #19865, #6516 ) ;
#2912 = EDGE_LOOP ( 'NONE', ( #12770, #8395, #17754, #1475 ) ) ;
#2913 = CARTESIAN_POINT ( 'NONE',  ( 0.000000000000000000, 91.70173545986537533, -12.13370160539944287 ) ) ;
#2914 =( NAMED_UNIT ( * ) SI_UNIT ( $, .STERADIAN. ) SOLID_ANGLE_UNIT ( ) );
#2915 = DIRECTION ( 'NONE',  ( -1.000000000000000000, 0.000000000000000000, 0.000000000000000000 ) ) ;
#2916 = ORIENTED_EDGE ( 'NONE', *, *, #13411, .F. ) ;
#2917 =( NAMED_UNIT ( * ) SI_UNIT ( $, .STERADIAN. ) SOLID_ANGLE_UNIT ( ) );
#2918 = ORIENTED_EDGE ( 'NONE', *, *, #7029, .T. ) ;
#2919 = AXIS2_PLACEMENT_3D ( 'NONE', #433, #19207, #4071 ) ;
#2920 = ORIENTED_EDGE ( 'NONE', *, *, #4236, .T. ) ;
#2921 = ORIENTED_EDGE ( 'NONE', *, *, #6673, .F. ) ;
#2922 = DIRECTION ( 'NONE',  ( 0.000000000000000000, 0.000000000000000000, 1.000000000000000000 ) ) ;
#2923 = LINE ( 'NONE', #14753, #12525 ) ;
#2924 = VECTOR ( 'NONE', #3901, 1000.000000000000000 ) ;
#2925 = ORIENTED_EDGE ( 'NONE', *, *, #12063, .T. ) ;
#2926 = CIRCLE ( 'NONE', #5759, 44.99999999999999289 ) ;
#2927 = CARTESIAN_POINT ( 'NONE',  ( 0.000000000000000000, 78.04699792498145428, 49.64978465107317618 ) ) ;
#2928 = CARTESIAN_POINT ( 'NONE',  ( -1.200000000000006617, 8.239576745513313235E-16, 6.728125000000022560 ) ) ;
#2929 = CARTESIAN_POINT ( 'NONE',  ( 0.000000000000000000, -41.21966518005896774, -82.80926399530329718 ) ) ;
#2930 = LINE ( 'NONE', #9549, #21668 ) ;
#2931 = DIRECTION ( 'NONE',  ( -1.000000000000000000, -0.000000000000000000, -0.000000000000000000 ) ) ;
#2932 = DIRECTION ( 'NONE',  ( -0.000000000000000000, -1.000000000000000000, -0.000000000000000000 ) ) ;
#2933 = CIRCLE ( 'NONE', #9994, 45.00000000000000711 ) ;
#2934 = ADVANCED_FACE ( 'NONE', ( #12956 ), #19708, .F. ) ;
#2935 = ORIENTED_EDGE ( 'NONE', *, *, #17047, .T. ) ;
#2936 = DIRECTION ( 'NONE',  ( -1.000000000000000000, -0.000000000000000000, 0.000000000000000000 ) ) ;
#2937 = CIRCLE ( 'NONE', #15277, 27.49900000000000233 ) ;
#2938 = LINE ( 'NONE', #18420, #13229 ) ;
#2939 = VERTEX_POINT ( 'NONE', #15947 ) ;
#2940 = EDGE_CURVE ( 'NONE', #13200, #733, #1252, .T. ) ;
#2941 = AXIS2_PLACEMENT_3D ( 'NONE', #7872, #19583, #13058 ) ;
#2942 = DIRECTION ( 'NONE',  ( -1.000000000000000000, -0.000000000000000000, -0.000000000000000000 ) ) ;
#2943 = VERTEX_POINT ( 'NONE', #2809 ) ;
#2944 = LINE ( 'NONE', #8249, #10912 ) ;
#2945 = CARTESIAN_POINT ( 'NONE',  ( 10.00000000000000000, -71.33759994381919967, -58.88447872959059026 ) ) ;
#2946 = ORIENTED_EDGE ( 'NONE', *, *, #3423, .T. ) ;
#2947 = LINE ( 'NONE', #9672, #7434 ) ;
#2948 = VECTOR ( 'NONE', #308, 1000.000000000000000 ) ;
#2949 = ORIENTED_EDGE ( 'NONE', *, *, #13942, .F. ) ;
#2950 = EDGE_LOOP ( 'NONE', ( #16762, #1736 ) ) ;
#2951 = CYLINDRICAL_SURFACE ( 'NONE', #10092, 5.000000000000000000 ) ;
#2952 = ORIENTED_EDGE ( 'NONE', *, *, #7432, .T. ) ;
#2953 = DIRECTION ( 'NONE',  ( 1.000000000000000000, 0.000000000000000000, 0.000000000000000000 ) ) ;
#2954 = AXIS2_PLACEMENT_3D ( 'NONE', #9861, #11642, #4673 ) ;
#2955 = LINE ( 'NONE', #9680, #13238 ) ;
#2956 = FACE_OUTER_BOUND ( 'NONE', #20735, .T. ) ;
#2957 = DIRECTION ( 'NONE',  ( 0.000000000000000000, 0.000000000000000000, 1.000000000000000000 ) ) ;
#2958 = AXIS2_PLACEMENT_3D ( 'NONE', #14858, #21595, #940 ) ;
#2959 = EDGE_CURVE ( 'NONE', #6824, #17849, #13593, .T. ) ;
#2960 = DIRECTION ( 'NONE',  ( -1.000000000000000000, -0.000000000000000000, 0.000000000000000000 ) ) ;
#2961 = EDGE_CURVE ( 'NONE', #5897, #12371, #3358, .T. ) ;
#2962 = LINE ( 'NONE', #18549, #10664 ) ;
#2963 = DIRECTION ( 'NONE',  ( -1.000000000000000000, -0.000000000000000000, -0.000000000000000000 ) ) ;
#2964 = CYLINDRICAL_SURFACE ( 'NONE', #10914, 92.50100000000000477 ) ;
#2965 = AXIS2_PLACEMENT_3D ( 'NONE', #4016, #709, #10641 ) ;
#2966 = CARTESIAN_POINT ( 'NONE',  ( 0.000000000000000000, 14.53731623274961571, -23.34226719384889748 ) ) ;
#2967 = DIRECTION ( 'NONE',  ( 1.000000000000000000, 0.000000000000000000, 0.000000000000000000 ) ) ;
#2968 = CIRCLE ( 'NONE', #5799, 88.00000000000000000 ) ;
#2969 = EDGE_LOOP ( 'NONE', ( #21371, #12356, #3685, #8578 ) ) ;
#2970 = ORIENTED_EDGE ( 'NONE', *, *, #1086, .T. ) ;
#2971 = ORIENTED_EDGE ( 'NONE', *, *, #17539, .F. ) ;
#2972 = EDGE_CURVE ( 'NONE', #9876, #1625, #4072, .T. ) ;
#2973 = VERTEX_POINT ( 'NONE', #3023 ) ;
#2974 = ORIENTED_EDGE ( 'NONE', *, *, #8864, .T. ) ;
#2975 = ADVANCED_FACE ( 'NONE', ( #3342 ), #11737, .F. ) ;
#2976 = CARTESIAN_POINT ( 'NONE',  ( 0.000000000000000000, 61.60362715319122628, -62.84101464466179721 ) ) ;
#2977 = VERTEX_POINT ( 'NONE', #16386 ) ;
#2978 = CARTESIAN_POINT ( 'NONE',  ( 0.000000000000000000, -45.60224695560626174, 80.47900393021710386 ) ) ;
#2979 = CIRCLE ( 'NONE', #14671, 6.866799999999992465 ) ;
#2980 = FACE_OUTER_BOUND ( 'NONE', #7219, .T. ) ;
#2981 = AXIS2_PLACEMENT_3D ( 'NONE', #4013, #8875, #17508 ) ;
#2982 = ADVANCED_FACE ( 'NONE', ( #16826 ), #11530, .F. ) ;
#2983 = CARTESIAN_POINT ( 'NONE',  ( 5.000000000000002665, -40.72878876293093242, -78.00747250042492453 ) ) ;
#2984 = DIRECTION ( 'NONE',  ( 1.000000000000000000, 0.000000000000000000, -0.000000000000000000 ) ) ;
#2985 = CYLINDRICAL_SURFACE ( 'NONE', #20700, 45.00000000000000000 ) ;
#2986 = EDGE_CURVE ( 'NONE', #10498, #2910, #1962, .T. ) ;
#2987 = AXIS2_PLACEMENT_3D ( 'NONE', #4892, #11636, #2192 ) ;
#2988 = DIRECTION ( 'NONE',  ( 0.000000000000000000, 0.2756373558169998295, -0.9612616959383187831 ) ) ;
#2989 = DIRECTION ( 'NONE',  ( 0.000000000000000000, 0.9993908270190956511, 0.03489949670250451497 ) ) ;
#2990 = EDGE_CURVE ( 'NONE', #11426, #6341, #6194, .T. ) ;
#2991 = ORIENTED_EDGE ( 'NONE', *, *, #4765, .F. ) ;
#2992 = DIRECTION ( 'NONE',  ( 0.000000000000000000, 0.7880107536067233465, -0.6156614753256567374 ) ) ;
#2993 = AXIS2_PLACEMENT_3D ( 'NONE', #2751, #11025, #12908 ) ;
#2994 = CIRCLE ( 'NONE', #21335, 32.00000000000000000 ) ;
#2995 = ORIENTED_EDGE ( 'NONE', *, *, #8197, .F. ) ;
#2996 = AXIS2_PLACEMENT_3D ( 'NONE', #1168, #17862, #12546 ) ;
#2997 = EDGE_LOOP ( 'NONE', ( #5307, #12866, #1469, #19939 ) ) ;
#2998 = EDGE_CURVE ( 'NONE', #5274, #9309, #4674, .T. ) ;
#2999 = CIRCLE ( 'NONE', #5835, 6.500000000000000000 ) ;
#3000 = CYLINDRICAL_SURFACE ( 'NONE', #4260, 12.00000000000000000 ) ;
#3001 = ORIENTED_EDGE ( 'NONE', *, *, #2200, .F. ) ;
#3002 = DIRECTION ( 'NONE',  ( -1.000000000000000000, -0.000000000000000000, -0.000000000000000000 ) ) ;
#3003 = ORIENTED_EDGE ( 'NONE', *, *, #10497, .F. ) ;
#3004 = EDGE_CURVE ( 'NONE', #1789, #8068, #20329, .T. ) ;
#3005 = ORIENTED_EDGE ( 'NONE', *, *, #17010, .F. ) ;
#3006 = AXIS2_PLACEMENT_3D ( 'NONE', #15101, #10243, #11794 ) ;
#3007 = APPLICATION_PROTOCOL_DEFINITION ( 'draft international standard', 'automotive_design', 1998, #14335 ) ;
#3008 = CARTESIAN_POINT ( 'NONE',  ( 123.0000000000000000, 0.000000000000000000, 25.00000000000000000 ) ) ;
#3009 = ORIENTED_EDGE ( 'NONE', *, *, #842, .F. ) ;
#3010 = VECTOR ( 'NONE', #18406, 1000.000000000000000 ) ;
#3011 = DIRECTION ( 'NONE',  ( 0.000000000000000000, 0.000000000000000000, 1.000000000000000000 ) ) ;
#3012 = FACE_OUTER_BOUND ( 'NONE', #2826, .T. ) ;
#3013 = EDGE_CURVE ( 'NONE', #15171, #3628, #2675, .T. ) ;
#3014 = DIRECTION ( 'NONE',  ( 0.000000000000000000, 0.000000000000000000, 1.000000000000000000 ) ) ;
#3015 = DIRECTION ( 'NONE',  ( 0.000000000000000000, -0.3420201433256757073, 0.9396926207859058744 ) ) ;
#3016 = AXIS2_PLACEMENT_3D ( 'NONE', #9863, #11413, #16710 ) ;
#3017 = AXIS2_PLACEMENT_3D ( 'NONE', #5503, #15650, #16996 ) ;
#3018 = CARTESIAN_POINT ( 'NONE',  ( 10.00000000000000000, -86.54587337002867287, -15.93147207947093946 ) ) ;
#3019 = AXIS2_PLACEMENT_3D ( 'NONE', #12186, #11973, #20264 ) ;
#3020 = DIRECTION ( 'NONE',  ( -1.000000000000000000, 0.000000000000000000, 0.000000000000000000 ) ) ;
#3021 = AXIS2_PLACEMENT_3D ( 'NONE', #275, #59, #17068 ) ;
#3022 = CARTESIAN_POINT ( 'NONE',  ( 0.000000000000000000, 18.94217447942559573, 85.93715160505956874 ) ) ;
#3023 = CARTESIAN_POINT ( 'NONE',  ( 10.49999999999999822, 1.285879139104720633E-15, 0.000000000000000000 ) ) ;
#3025 = CIRCLE ( 'NONE', #12536, 88.00000000000000000 ) ;
#3024 = CARTESIAN_POINT ( 'NONE',  ( 1.500000000000000000, -7.000000000000000000, 15.00000000000000000 ) ) ;
#3026 = ADVANCED_FACE ( 'NONE', ( #6358 ), #19921, .F. ) ;
#3027 = ORIENTED_EDGE ( 'NONE', *, *, #14112, .F. ) ;
#3028 = VERTEX_POINT ( 'NONE', #36 ) ;
#3029 = DIRECTION ( 'NONE',  ( 1.000000000000000000, 0.000000000000000000, 0.000000000000000000 ) ) ;
#3030 = CARTESIAN_POINT ( 'NONE',  ( 0.000000000000000000, 0.000000000000000000, 15.00000000000000000 ) ) ;
#3031 = ORIENTED_EDGE ( 'NONE', *, *, #2391, .F. ) ;
#3032 = AXIS2_PLACEMENT_3D ( 'NONE', #3489, #9074, #10228 ) ;
#3033 = CYLINDRICAL_SURFACE ( 'NONE', #21720, 44.99999999999999289 ) ;
#3034 = AXIS2_PLACEMENT_3D ( 'NONE', #390, #3813, #13860 ) ;
#3035 = ORIENTED_EDGE ( 'NONE', *, *, #17571, .F. ) ;
#3036 = AXIS2_PLACEMENT_3D ( 'NONE', #9743, #18052, #2904 ) ;
#3037 = VECTOR ( 'NONE', #12712, 1000.000000000000000 ) ;
#3038 = ORIENTED_EDGE ( 'NONE', *, *, #11898, .F. ) ;
#3039 = ORIENTED_EDGE ( 'NONE', *, *, #16740, .F. ) ;
#3040 = EDGE_LOOP ( 'NONE', ( #15423, #1417, #15958, #16737 ) ) ;
#3041 = CARTESIAN_POINT ( 'NONE',  ( -8.900000000000018119, 0.000000000000000000, 0.000000000000000000 ) ) ;
#3042 = LINE ( 'NONE', #1483, #8653 ) ;
#3043 = EDGE_LOOP ( 'NONE', ( #18237, #16756, #16895, #13114 ) ) ;
#3044 = EDGE_CURVE ( 'NONE', #4876, #7568, #16085, .T. ) ;
#3045 = FACE_OUTER_BOUND ( 'NONE', #4364, .T. ) ;
#3046 = LINE ( 'NONE', #15073, #18985 ) ;
#3047 = CARTESIAN_POINT ( 'NONE',  ( -10.00000000000000000, 0.000000000000000000, 0.000000000000000000 ) ) ;
#3048 = DIRECTION ( 'NONE',  ( 0.000000000000000000, -0.8290375725550350738, -0.5591929034707566748 ) ) ;
#3049 = CARTESIAN_POINT ( 'NONE',  ( 0.000000000000000000, 0.000000000000000000, 0.000000000000000000 ) ) ;
#3050 = CARTESIAN_POINT ( 'NONE',  ( -1.500000000000000000, -7.000000000000000000, 15.00000000000000000 ) ) ;
#3051 = UNCERTAINTY_MEASURE_WITH_UNIT (LENGTH_MEASURE( 1.000000000000000082E-05 ), #12039, 'distance_accuracy_value', 'NONE');
#3052 = ORIENTED_EDGE ( 'NONE', *, *, #21055, .T. ) ;
#3053 = AXIS2_PLACEMENT_3D ( 'NONE', #11641, #7997, #4787 ) ;
#3054 = FACE_OUTER_BOUND ( 'NONE', #19989, .T. ) ;
#3055 = FACE_OUTER_BOUND ( 'NONE', #11175, .T. ) ;
#3056 = EDGE_LOOP ( 'NONE', ( #6134, #18407, #21026, #15954 ) ) ;
#3057 = DIRECTION ( 'NONE',  ( 0.000000000000000000, 0.3420201433256631063, 0.9396926207859105373 ) ) ;
#3058 = ORIENTED_EDGE ( 'NONE', *, *, #415, .T. ) ;
#3059 = FACE_OUTER_BOUND ( 'NONE', #19879, .T. ) ;
#3060 = DIRECTION ( 'NONE',  ( -1.000000000000000000, 0.000000000000000000, 0.000000000000000000 ) ) ;
#3061 = VERTEX_POINT ( 'NONE', #11306 ) ;
#3062 = DIRECTION ( 'NONE',  ( 0.000000000000000000, 0.000000000000000000, -1.000000000000000000 ) ) ;
#3063 = ORIENTED_EDGE ( 'NONE', *, *, #14328, .T. ) ;
#3064 = CIRCLE ( 'NONE', #21409, 45.00000000000000000 ) ;
#3065 = CIRCLE ( 'NONE', #4834, 126.5000000000000000 ) ;
#3066 = ORIENTED_EDGE ( 'NONE', *, *, #13794, .T. ) ;
#3067 = CARTESIAN_POINT ( 'NONE',  ( 10.00000000000000000, -84.80486432185219314, 36.94008646920367056 ) ) ;
#3068 = AXIS2_PLACEMENT_3D ( 'NONE', #137, #20476, #13938 ) ;
#3069 = ORIENTED_EDGE ( 'NONE', *, *, #15686, .F. ) ;
#3070 = FACE_OUTER_BOUND ( 'NONE', #2236, .T. ) ;
#3071 = DIRECTION ( 'NONE',  ( -1.000000000000000000, 0.000000000000000000, 0.000000000000000000 ) ) ;
#3072 = CARTESIAN_POINT ( 'NONE',  ( 0.000000000000000000, -65.83713140174687339, -58.39068529131263574 ) ) ;
#3073 = CARTESIAN_POINT ( 'NONE',  ( 1.139999999999997460, 5.633200000000004870, 0.000000000000000000 ) ) ;
#3074 = DIRECTION ( 'NONE',  ( -1.000000000000000000, -0.000000000000000000, 0.000000000000000000 ) ) ;
#3075 = ADVANCED_FACE ( 'NONE', ( #21684, #6574 ), #6687, .F. ) ;
#3076 = LINE ( 'NONE', #16561, #8043 ) ;
#3077 = CARTESIAN_POINT ( 'NONE',  ( -10.00000000000000000, 0.000000000000000000, 0.000000000000000000 ) ) ;
#3078 = CARTESIAN_POINT ( 'NONE',  ( 10.00000000000000000, -83.35585896458606214, -16.94078559808036033 ) ) ;
#3079 = CARTESIAN_POINT ( 'NONE',  ( 10.00000000000000000, 27.87320266523671819, -88.20158487341731757 ) ) ;
#3080 = AXIS2_PLACEMENT_3D ( 'NONE', #15135, #10602, #12044 ) ;
#3081 = DIRECTION ( 'NONE',  ( 0.000000000000000000, 0.7431448254773954654, -0.6691306063588569053 ) ) ;
#3082 = AXIS2_PLACEMENT_3D ( 'NONE', #5719, #7810, #14329 ) ;
#3083 = AXIS2_PLACEMENT_3D ( 'NONE', #10700, #7402, #4729 ) ;
#3084 = DIRECTION ( 'NONE',  ( -1.000000000000000000, -0.000000000000000000, -0.000000000000000000 ) ) ;
#3085 = ORIENTED_EDGE ( 'NONE', *, *, #321, .T. ) ;
#3086 = VERTEX_POINT ( 'NONE', #3130 ) ;
#3087 = ORIENTED_EDGE ( 'NONE', *, *, #11259, .T. ) ;
#3088 = ORIENTED_EDGE ( 'NONE', *, *, #422, .F. ) ;
#3089 = EDGE_CURVE ( 'NONE', #10281, #7717, #13288, .T. ) ;
#3090 = ORIENTED_EDGE ( 'NONE', *, *, #18408, .F. ) ;
#3091 = DIRECTION ( 'NONE',  ( -1.000000000000000000, 0.000000000000000000, -0.000000000000000000 ) ) ;
#3092 = AXIS2_PLACEMENT_3D ( 'NONE', #19431, #12690, #2198 ) ;
#3093 = ORIENTED_EDGE ( 'NONE', *, *, #3131, .T. ) ;
#3094 = FACE_OUTER_BOUND ( 'NONE', #8793, .T. ) ;
#3095 = AXIS2_PLACEMENT_3D ( 'NONE', #17633, #21045, #12413 ) ;
#3096 = FACE_BOUND ( 'NONE', #14025, .T. ) ;
#3097 = EDGE_CURVE ( 'NONE', #6505, #2865, #8323, .T. ) ;
#3098 = DIRECTION ( 'NONE',  ( 1.000000000000000000, -0.000000000000000000, -0.000000000000000000 ) ) ;
#3099 = CARTESIAN_POINT ( 'NONE',  ( 0.000000000000000000, 64.66851233300799606, -55.25552418572899427 ) ) ;
#3100 = CARTESIAN_POINT ( 'NONE',  ( 10.00000000000000000, 1.592605004252791279, 28.14575649959894932 ) ) ;
#3101 = DIRECTION ( 'NONE',  ( 0.000000000000000000, 0.000000000000000000, 1.000000000000000000 ) ) ;
#3102 = EDGE_CURVE ( 'NONE', #20413, #11578, #1629, .T. ) ;
#3103 = CARTESIAN_POINT ( 'NONE',  ( 10.00000000000000000, 0.000000000000000000, 0.000000000000000000 ) ) ;
#3104 = VERTEX_POINT ( 'NONE', #20148 ) ;
#3105 = DIRECTION ( 'NONE',  ( 1.000000000000000000, 0.000000000000000000, 0.000000000000000000 ) ) ;
#3106 = CIRCLE ( 'NONE', #11585, 11.99999999999999822 ) ;
#3107 = ORIENTED_EDGE ( 'NONE', *, *, #20938, .T. ) ;
#3108 = ORIENTED_EDGE ( 'NONE', *, *, #13816, .T. ) ;
#3109 = CARTESIAN_POINT ( 'NONE',  ( 10.00000000000000000, 2.208823992045340301, -85.03123271466934341 ) ) ;
#3110 = EDGE_CURVE ( 'NONE', #21233, #12524, #11845, .T. ) ;
#3111 = ORIENTED_EDGE ( 'NONE', *, *, #10788, .T. ) ;
#3112 = EDGE_CURVE ( 'NONE', #15636, #8019, #10622, .T. ) ;
#3113 = ADVANCED_FACE ( 'NONE', ( #17370 ), #15263, .T. ) ;
#3114 = DIRECTION ( 'NONE',  ( 0.000000000000000000, 0.000000000000000000, 1.000000000000000000 ) ) ;
#3115 = ORIENTED_EDGE ( 'NONE', *, *, #17299, .T. ) ;
#3116 = ORIENTED_EDGE ( 'NONE', *, *, #1649, .T. ) ;
#3117 = DIRECTION ( 'NONE',  ( -1.000000000000000000, 0.000000000000000000, -0.000000000000000000 ) ) ;
#3118 = EDGE_CURVE ( 'NONE', #4988, #11544, #9714, .T. ) ;
#3119 = EDGE_LOOP ( 'NONE', ( #17057, #6468, #9490, #21620 ) ) ;
#3120 = LINE ( 'NONE', #432, #2293 ) ;
#3121 = FACE_OUTER_BOUND ( 'NONE', #21077, .T. ) ;
#3122 = VECTOR ( 'NONE', #2648, 1000.000000000000000 ) ;
#3123 = FACE_OUTER_BOUND ( 'NONE', #9898, .T. ) ;
#3124 = DIRECTION ( 'NONE',  ( 0.000000000000000000, 0.1391731009600657987, -0.9902680687415702510 ) ) ;
#3125 = VECTOR ( 'NONE', #14548, 1000.000000000000000 ) ;
#3126 = CARTESIAN_POINT ( 'NONE',  ( 10.00000000000000000, 0.000000000000000000, 0.000000000000000000 ) ) ;
#3127 = AXIS2_PLACEMENT_3D ( 'NONE', #6540, #19786, #11378 ) ;
#3128 = AXIS2_PLACEMENT_3D ( 'NONE', #1453, #13271, #20024 ) ;
#3129 = FACE_OUTER_BOUND ( 'NONE', #7443, .T. ) ;
#3130 = CARTESIAN_POINT ( 'NONE',  ( 0.000000000000000000, -15.32665449651985590, 91.22241316115413667 ) ) ;
#3131 = EDGE_CURVE ( 'NONE', #2159, #15310, #218, .T. ) ;
#3132 = CARTESIAN_POINT ( 'NONE',  ( -10.00000000000000000, 0.000000000000000000, 0.000000000000000000 ) ) ;
#3133 = EDGE_LOOP ( 'NONE', ( #399, #724, #2117, #352 ) ) ;
#3134 = EDGE_CURVE ( 'NONE', #16531, #5051, #6535, .T. ) ;
#3135 = ADVANCED_FACE ( 'NONE', ( #10512 ), #16031, .T. ) ;
#3136 = CARTESIAN_POINT ( 'NONE',  ( 10.00000000000000000, 0.000000000000000000, 0.000000000000000000 ) ) ;
#3137 = CIRCLE ( 'NONE', #17957, 92.50100000000000477 ) ;
#3138 = DIRECTION ( 'NONE',  ( 0.000000000000000000, 0.000000000000000000, 1.000000000000000000 ) ) ;
#3139 = VERTEX_POINT ( 'NONE', #11966 ) ;
#3140 = CIRCLE ( 'NONE', #4201, 88.00000000000000000 ) ;
#3141 = FACE_OUTER_BOUND ( 'NONE', #10285, .T. ) ;
#3142 = AXIS2_PLACEMENT_3D ( 'NONE', #9155, #3868, #5966 ) ;
#3143 = ORIENTED_EDGE ( 'NONE', *, *, #4563, .F. ) ;
#3144 = ORIENTED_EDGE ( 'NONE', *, *, #8827, .T. ) ;
#3145 = FACE_OUTER_BOUND ( 'NONE', #265, .T. ) ;
#3146 = ADVANCED_FACE ( 'NONE', ( #12173 ), #20253, .F. ) ;
#3147 = ORIENTED_EDGE ( 'NONE', *, *, #6494, .F. ) ;
#3148 = ORIENTED_EDGE ( 'NONE', *, *, #17662, .F. ) ;
#3149 = DIRECTION ( 'NONE',  ( 1.000000000000000000, 0.000000000000000000, 0.000000000000000000 ) ) ;
#3150 = CARTESIAN_POINT ( 'NONE',  ( 10.00000000000000000, 0.000000000000000000, 0.000000000000000000 ) ) ;
#3151 = EDGE_LOOP ( 'NONE', ( #2291, #12878, #13374, #13037 ) ) ;
#3152 = VECTOR ( 'NONE', #365, 1000.000000000000000 ) ;
#3153 = CARTESIAN_POINT ( 'NONE',  ( 0.000000000000000000, 0.000000000000000000, 0.000000000000000000 ) ) ;
#3154 = CARTESIAN_POINT ( 'NONE',  ( 10.00000000000000000, -40.72878876293093242, -78.00747250042492453 ) ) ;
#3155 = DIRECTION ( 'NONE',  ( 1.000000000000000000, 0.000000000000000000, 0.000000000000000000 ) ) ;
#3156 = DIRECTION ( 'NONE',  ( 0.000000000000000000, 0.000000000000000000, 1.000000000000000000 ) ) ;
#3157 = DIRECTION ( 'NONE',  ( 0.000000000000000000, -0.9945218953682722907, -0.1045284632676634906 ) ) ;
#3158 = DIRECTION ( 'NONE',  ( 0.000000000000000000, 0.000000000000000000, 1.000000000000000000 ) ) ;
#3159 = EDGE_CURVE ( 'NONE', #12184, #6987, #18169, .T. ) ;
#3160 = AXIS2_PLACEMENT_3D ( 'NONE', #4474, #6698, #21491 ) ;
#3161 = CIRCLE ( 'NONE', #15503, 88.00000000000000000 ) ;
#3162 = ORIENTED_EDGE ( 'NONE', *, *, #10633, .F. ) ;
#3163 = EDGE_CURVE ( 'NONE', #14101, #13181, #251, .T. ) ;
#3164 = CIRCLE ( 'NONE', #5285, 88.00000000000000000 ) ;
#3165 = DIRECTION ( 'NONE',  ( 1.000000000000000000, 0.000000000000000000, 0.000000000000000000 ) ) ;
#3166 = DIRECTION ( 'NONE',  ( 0.000000000000000000, -0.8290375725550350738, -0.5591929034707566748 ) ) ;
#3167 = ORIENTED_EDGE ( 'NONE', *, *, #7876, .T. ) ;
#3168 = EDGE_CURVE ( 'NONE', #14063, #16061, #15497, .T. ) ;
#3169 = ADVANCED_FACE ( 'NONE', ( #10296 ), #18600, .T. ) ;
#3170 = DIRECTION ( 'NONE',  ( 1.000000000000000000, -0.000000000000000000, -0.000000000000000000 ) ) ;
#3171 = EDGE_LOOP ( 'NONE', ( #8883, #4615, #2916, #1414 ) ) ;
#3172 = CYLINDRICAL_SURFACE ( 'NONE', #7394, 11.99999999999999822 ) ;
#3173 = DIRECTION ( 'NONE',  ( -1.000000000000000000, -0.000000000000000000, -0.000000000000000000 ) ) ;
#3174 = ORIENTED_EDGE ( 'NONE', *, *, #5865, .T. ) ;
#3175 = CARTESIAN_POINT ( 'NONE',  ( 10.00000000000000000, 0.000000000000000000, 0.000000000000000000 ) ) ;
#3176 = ORIENTED_EDGE ( 'NONE', *, *, #17732, .T. ) ;
#3177 = ORIENTED_EDGE ( 'NONE', *, *, #18439, .F. ) ;
#3178 = CIRCLE ( 'NONE', #13759, 88.00000000000000000 ) ;
#3179 = CARTESIAN_POINT ( 'NONE',  ( 0.000000000000000000, 100.0000000000000000, 0.000000000000000000 ) ) ;
#3180 = VECTOR ( 'NONE', #18844, 1000.000000000000000 ) ;
#3181 = EDGE_LOOP ( 'NONE', ( #21643, #21647, #3093, #2314 ) ) ;
#3182 = CARTESIAN_POINT ( 'NONE',  ( 0.000000000000000000, 66.01871308925461790, 64.79170103523043167 ) ) ;
#3183 = CARTESIAN_POINT ( 'NONE',  ( 10.00000000000000000, 27.26034713664087406, 7.182859710736605230 ) ) ;
#3184 = CARTESIAN_POINT ( 'NONE',  ( 10.00000000000000000, 9.646732466566502850, -84.51112348751837544 ) ) ;
#3185 = CARTESIAN_POINT ( 'NONE',  ( 0.000000000000000000, 8.925965667928872804, 92.06933331948788179 ) ) ;
#3186 = CARTESIAN_POINT ( 'NONE',  ( 10.00000000000000000, 61.33825423015778711, -69.23910433415882437 ) ) ;
#3187 = CARTESIAN_POINT ( 'NONE',  ( -1.400000000000000577, 0.000000000000000000, 0.000000000000000000 ) ) ;
#3188 = DIRECTION ( 'NONE',  ( -1.000000000000000000, -0.000000000000000000, -0.000000000000000000 ) ) ;
#3189 = DIRECTION ( 'NONE',  ( 1.000000000000000000, 0.000000000000000000, -0.000000000000000000 ) ) ;
#3190 = CARTESIAN_POINT ( 'NONE',  ( 10.00000000000000000, -21.69483248597433089, 16.89761061231773454 ) ) ;
#3191 = AXIS2_PLACEMENT_3D ( 'NONE', #7977, #19251, #6006 ) ;
#3192 = DIRECTION ( 'NONE',  ( 0.000000000000000000, 0.000000000000000000, 1.000000000000000000 ) ) ;
#3193 = ORIENTED_EDGE ( 'NONE', *, *, #20460, .T. ) ;
#3194 = ORIENTED_EDGE ( 'NONE', *, *, #19459, .F. ) ;
#3195 = ORIENTED_EDGE ( 'NONE', *, *, #14599, .F. ) ;
#3196 = ORIENTED_EDGE ( 'NONE', *, *, #17025, .T. ) ;
#3197 = EDGE_LOOP ( 'NONE', ( #5402, #15087, #15019, #15960 ) ) ;
#3198 = CARTESIAN_POINT ( 'NONE',  ( 10.00000000000000000, 9.366510754379572035, -25.85466064925416774 ) ) ;
#3199 = EDGE_LOOP ( 'NONE', ( #12894, #19274, #1452, #20814 ) ) ;
#3200 = CYLINDRICAL_SURFACE ( 'NONE', #17740, 92.50100000000000477 ) ;
#3201 = AXIS2_PLACEMENT_3D ( 'NONE', #21522, #6399, #12773 ) ;
#3202 = CARTESIAN_POINT ( 'NONE',  ( 10.00000000000000000, 71.33759994381962599, 58.88447872959010709 ) ) ;
#3203 = CYLINDRICAL_SURFACE ( 'NONE', #4688, 88.00000000000000000 ) ;
#3204 = DIRECTION ( 'NONE',  ( 1.000000000000000000, 0.000000000000000000, 0.000000000000000000 ) ) ;
#3205 =( LENGTH_UNIT ( ) NAMED_UNIT ( * ) SI_UNIT ( .MILLI., .METRE. ) );
#3206 = CARTESIAN_POINT ( 'NONE',  ( 10.00000000000000000, 0.000000000000000000, 0.000000000000000000 ) ) ;
#3207 = CARTESIAN_POINT ( 'NONE',  ( 10.00000000000000000, 46.93287725819874368, -70.94007663282398823 ) ) ;
#3208 = VECTOR ( 'NONE', #6810, 1000.000000000000000 ) ;
#3209 = EDGE_CURVE ( 'NONE', #12163, #4259, #7239, .T. ) ;
#3210 = VERTEX_POINT ( 'NONE', #15597 ) ;
#3211 = DIRECTION ( 'NONE',  ( -1.000000000000000000, -0.000000000000000000, -0.000000000000000000 ) ) ;
#3212 = ORIENTED_EDGE ( 'NONE', *, *, #19486, .F. ) ;
#3213 = EDGE_CURVE ( 'NONE', #12268, #2625, #10048, .T. ) ;
#3214 = VERTEX_POINT ( 'NONE', #8537 ) ;
#3215 = DIRECTION ( 'NONE',  ( 0.000000000000000000, 1.224646799147353207E-16, 1.000000000000000000 ) ) ;
#3216 = VERTEX_POINT ( 'NONE', #5338 ) ;
#3217 = DIRECTION ( 'NONE',  ( -1.000000000000000000, -0.000000000000000000, -0.000000000000000000 ) ) ;
#3218 = EDGE_LOOP ( 'NONE', ( #15798, #14144, #4257, #3451 ) ) ;
#3219 = ORIENTED_EDGE ( 'NONE', *, *, #6093, .F. ) ;
#3220 = PRODUCT_CONTEXT ( 'NONE', #1631, 'mechanical' ) ;
#3221 = CYLINDRICAL_SURFACE ( 'NONE', #7679, 113.8250000000000171 ) ;
#3222 = VERTEX_POINT ( 'NONE', #17271 ) ;
#3223 = LINE ( 'NONE', #15670, #21691 ) ;
#3224 = CARTESIAN_POINT ( 'NONE',  ( 5.000000000000000000, 30.24235385705238244, 10.45944707835118237 ) ) ;
#3226 = CIRCLE ( 'NONE', #1461, 44.99999999999998579 ) ;
#3225 = FACE_BOUND ( 'NONE', #21726, .T. ) ;
#3227 = DIRECTION ( 'NONE',  ( 1.000000000000000000, 0.000000000000000000, 0.000000000000000000 ) ) ;
#3228 = CARTESIAN_POINT ( 'NONE',  ( 10.00000000000000000, 61.71252885873465033, -58.53847642588533517 ) ) ;
#3229 =( GEOMETRIC_REPRESENTATION_CONTEXT ( 3 ) GLOBAL_UNCERTAINTY_ASSIGNED_CONTEXT ( ( #18310 ) ) GLOBAL_UNIT_ASSIGNED_CONTEXT ( ( #3244, #5015, #3469 ) ) REPRESENTATION_CONTEXT ( 'NONE', 'WORKASPACE' ) );
#3230 = CARTESIAN_POINT ( 'NONE',  ( 0.000000000000000000, 100.0000000000000000, -5.000000000000000000 ) ) ;
#3231 = DIRECTION ( 'NONE',  ( 0.000000000000000000, -0.5877852522924631451, -0.8090169943749545567 ) ) ;
#3232 = DIRECTION ( 'NONE',  ( -1.000000000000000000, 0.000000000000000000, -0.000000000000000000 ) ) ;
#3233 = ADVANCED_FACE ( 'NONE', ( #12065 ), #17158, .F. ) ;
#3234 = EDGE_CURVE ( 'NONE', #20275, #1388, #18810, .T. ) ;
#3235 = EDGE_CURVE ( 'NONE', #5871, #1245, #3866, .T. ) ;
#3236 = ORIENTED_EDGE ( 'NONE', *, *, #16937, .F. ) ;
#3237 = ADVANCED_FACE ( 'NONE', ( #12280 ), #21227, .T. ) ;
#3238 = CARTESIAN_POINT ( 'NONE',  ( 10.00000000000000000, 0.000000000000000000, 0.000000000000000000 ) ) ;
#3239 = LINE ( 'NONE', #16833, #17998 ) ;
#3240 = ORIENTED_EDGE ( 'NONE', *, *, #3893, .T. ) ;
#3241 = PRODUCT_DEFINITION_FORMATION_WITH_SPECIFIED_SOURCE ( 'ANY', '', #18138, .NOT_KNOWN. ) ;
#3242 = LINE ( 'NONE', #21695, #11124 ) ;
#3243 = EDGE_LOOP ( 'NONE', ( #3144, #8652, #14945, #7704 ) ) ;
#3244 =( LENGTH_UNIT ( ) NAMED_UNIT ( * ) SI_UNIT ( .MILLI., .METRE. ) );
#3245 = EDGE_CURVE ( 'NONE', #7456, #18401, #20883, .T. ) ;
#3246 = ORIENTED_EDGE ( 'NONE', *, *, #4484, .F. ) ;
#3247 = PLANE ( 'NONE',  #11760 ) ;
#3248 = VERTEX_POINT ( 'NONE', #1114 ) ;
#3249 = ORIENTED_EDGE ( 'NONE', *, *, #7613, .T. ) ;
#3250 = CARTESIAN_POINT ( 'NONE',  ( -9.999999999999998224, 0.000000000000000000, 15.00000000000000000 ) ) ;
#3251 = DIRECTION ( 'NONE',  ( 0.000000000000000000, -0.9993908270190954291, -0.03489949670251119018 ) ) ;
#3252 = ORIENTED_EDGE ( 'NONE', *, *, #13768, .F. ) ;
#3253 = EDGE_CURVE ( 'NONE', #3881, #6503, #15821, .T. ) ;
#3254 = AXIS2_PLACEMENT_3D ( 'NONE', #14479, #11043, #17794 ) ;
#3255 = DIRECTION ( 'NONE',  ( 0.000000000000000000, 0.000000000000000000, 1.000000000000000000 ) ) ;
#3256 = CYLINDRICAL_SURFACE ( 'NONE', #17531, 123.0000000000000000 ) ;
#3257 = DIRECTION ( 'NONE',  ( 0.000000000000000000, 0.000000000000000000, 1.000000000000000000 ) ) ;
#3258 = CARTESIAN_POINT ( 'NONE',  ( 0.000000000000000000, -3.786343810537759147, 27.23708136986050832 ) ) ;
#3259 = DIRECTION ( 'NONE',  ( -1.000000000000000000, -0.000000000000000000, 0.000000000000000000 ) ) ;
#3260 = CARTESIAN_POINT ( 'NONE',  ( 10.00000000000000000, 0.000000000000000000, 0.000000000000000000 ) ) ;
#3261 = UNCERTAINTY_MEASURE_WITH_UNIT (LENGTH_MEASURE( 1.000000000000000082E-05 ), #9086, 'distance_accuracy_value', 'NONE');
#3262 = EDGE_CURVE ( 'NONE', #4329, #2849, #18630, .T. ) ;
#3263 = EDGE_LOOP ( 'NONE', ( #9431, #5750, #15890, #9883 ) ) ;
#3264 = CARTESIAN_POINT ( 'NONE',  ( 10.00000000000000000, -21.98203405400942856, -17.64965094506566246 ) ) ;
#3265 = EDGE_CURVE ( 'NONE', #15149, #8047, #12912, .T. ) ;
#3266 = CIRCLE ( 'NONE', #8901, 105.0992000000000104 ) ;
#3267 = CYLINDRICAL_SURFACE ( 'NONE', #19957, 44.99999999999999289 ) ;
#3268 = VERTEX_POINT ( 'NONE', #6098 ) ;
#3269 = DIRECTION ( 'NONE',  ( 0.000000000000000000, 0.000000000000000000, 1.000000000000000000 ) ) ;
#3270 = ORIENTED_EDGE ( 'NONE', *, *, #16507, .F. ) ;
#3271 = VECTOR ( 'NONE', #7961, 1000.000000000000000 ) ;
#3272 = AXIS2_PLACEMENT_3D ( 'NONE', #8505, #18357, #3535 ) ;
#3273 = CARTESIAN_POINT ( 'NONE',  ( 0.000000000000000000, 0.000000000000000000, 0.000000000000000000 ) ) ;
#3274 = DIRECTION ( 'NONE',  ( 1.000000000000000000, 0.000000000000000000, 0.000000000000000000 ) ) ;
#3275 = ORIENTED_EDGE ( 'NONE', *, *, #12162, .T. ) ;
#3276 = CIRCLE ( 'NONE', #13141, 32.00000000000000000 ) ;
#3277 = CARTESIAN_POINT ( 'NONE',  ( 10.00000000000000000, -68.36541360927154187, -50.60987712331774446 ) ) ;
#3278 = ADVANCED_FACE ( 'NONE', ( #21122 ), #19130, .T. ) ;
#3279 = ORIENTED_EDGE ( 'NONE', *, *, #20460, .F. ) ;
#3280 = ORIENTED_EDGE ( 'NONE', *, *, #12179, .F. ) ;
#3281 = FACE_OUTER_BOUND ( 'NONE', #20162, .T. ) ;
#3282 = EDGE_CURVE ( 'NONE', #3214, #16126, #5883, .T. ) ;
#3283 = VERTEX_POINT ( 'NONE', #14258 ) ;
#3284 = LINE ( 'NONE', #1309, #9849 ) ;
#3285 = AXIS2_PLACEMENT_3D ( 'NONE', #20220, #6755, #18574 ) ;
#3286 = CARTESIAN_POINT ( 'NONE',  ( 10.00000000000000000, 25.48117629651203941, -10.33947075754235989 ) ) ;
#3287 = DIRECTION ( 'NONE',  ( 0.000000000000000000, 0.000000000000000000, -1.000000000000000000 ) ) ;
#3288 = CARTESIAN_POINT ( 'NONE',  ( -8.000000000000007105, 0.000000000000000000, 0.000000000000000000 ) ) ;
#3289 = ADVANCED_FACE ( 'NONE', ( #4432 ), #14490, .T. ) ;
#3290 = EDGE_CURVE ( 'NONE', #282, #21704, #809, .T. ) ;
#3291 = AXIS2_PLACEMENT_3D ( 'NONE', #8834, #341, #7401 ) ;
#3292 = AXIS2_PLACEMENT_3D ( 'NONE', #21415, #16111, #12682 ) ;
#3293 = LINE ( 'NONE', #18547, #10846 ) ;
#3294 = DIRECTION ( 'NONE',  ( 1.000000000000000000, 0.000000000000000000, 0.000000000000000000 ) ) ;
#3295 = VECTOR ( 'NONE', #10853, 1000.000000000000000 ) ;
#3296 = CARTESIAN_POINT ( 'NONE',  ( 10.00000000000000000, 0.000000000000000000, 0.000000000000000000 ) ) ;
#3297 = EDGE_CURVE ( 'NONE', #15150, #481, #20716, .T. ) ;
#3298 = CARTESIAN_POINT ( 'NONE',  ( 0.000000000000000000, 0.000000000000000000, 0.000000000000000000 ) ) ;
#3299 = CARTESIAN_POINT ( 'NONE',  ( 10.00000000000000000, -6.063030049134860100, -31.42037024962131397 ) ) ;
#3300 = VERTEX_POINT ( 'NONE', #14049 ) ;
#3301 = CIRCLE ( 'NONE', #5056, 92.50100000000000477 ) ;
#3302 = CARTESIAN_POINT ( 'NONE',  ( 5.000000000000000888, 28.00896854772013000, -15.47571261340895887 ) ) ;
#3303 = ORIENTED_EDGE ( 'NONE', *, *, #19060, .F. ) ;
#3304 = DIRECTION ( 'NONE',  ( 0.000000000000000000, -0.4067366430758070917, 0.9135454576425978690 ) ) ;
#3305 = ORIENTED_EDGE ( 'NONE', *, *, #20447, .F. ) ;
#3306 = CIRCLE ( 'NONE', #18119, 1.100000000000003642 ) ;
#3307 = ORIENTED_EDGE ( 'NONE', *, *, #11063, .T. ) ;
#3308 = ORIENTED_EDGE ( 'NONE', *, *, #20133, .T. ) ;
#3309 = DIRECTION ( 'NONE',  ( -1.000000000000000000, 0.000000000000000000, 0.000000000000000000 ) ) ;
#3310 = ORIENTED_EDGE ( 'NONE', *, *, #1774, .F. ) ;
#3311 = CYLINDRICAL_SURFACE ( 'NONE', #3617, 5.612499999999999822 ) ;
#3312 = DIRECTION ( 'NONE',  ( 0.000000000000000000, -0.2756373558170062132, 0.9612616959383166737 ) ) ;
#3313 = EDGE_CURVE ( 'NONE', #282, #17660, #2778, .T. ) ;
#3314 = CIRCLE ( 'NONE', #15657, 45.00000000000000711 ) ;
#3315 = DIRECTION ( 'NONE',  ( 0.000000000000000000, 0.2079116908177532919, 0.9781476007338070211 ) ) ;
#3316 = CYLINDRICAL_SURFACE ( 'NONE', #21768, 115.1000000000000227 ) ;
#3317 = CARTESIAN_POINT ( 'NONE',  ( 10.00000000000000000, -78.01214607583727911, -33.90124636420193838 ) ) ;
#3318 = DIRECTION ( 'NONE',  ( 0.000000000000000000, -0.6427876096865299260, -0.7660444431189857850 ) ) ;
#3319 = ORIENTED_EDGE ( 'NONE', *, *, #7155, .T. ) ;
#3320 = PRODUCT_DEFINITION_SHAPE ( 'NONE', 'NONE',  #101 ) ;
#3321 = TOROIDAL_SURFACE ( 'NONE', #9296, 114.9007999999999896, 0.2041999999999998816 ) ;
#3322 = CARTESIAN_POINT ( 'NONE',  ( 0.000000000000000000, 2.208823992045340301, -85.03123271466934341 ) ) ;
#3323 = ORIENTED_EDGE ( 'NONE', *, *, #7840, .F. ) ;
#3324 = VERTEX_POINT ( 'NONE', #7428 ) ;
#3325 = DIRECTION ( 'NONE',  ( -1.000000000000000000, 0.000000000000000000, 0.000000000000000000 ) ) ;
#3326 = VERTEX_POINT ( 'NONE', #2339 ) ;
#3327 = CARTESIAN_POINT ( 'NONE',  ( 10.00000000000000000, -77.39385041987125646, -35.28996114464684553 ) ) ;
#3328 = ORIENTED_EDGE ( 'NONE', *, *, #20629, .T. ) ;
#3329 = ORIENTED_EDGE ( 'NONE', *, *, #9020, .T. ) ;
#3330 = ITEM_DEFINED_TRANSFORMATION ( 'NONE', 'NONE', #3942,  #15567 ) ;
#3331 = AXIS2_PLACEMENT_3D ( 'NONE', #2599, #5706, #15966 ) ;
#3332 = CARTESIAN_POINT ( 'NONE',  ( 10.00000000000000000, 23.57863763525741874, -15.45211464167639548 ) ) ;
#3333 = ORIENTED_EDGE ( 'NONE', *, *, #16380, .T. ) ;
#3334 = EDGE_CURVE ( 'NONE', #6248, #18295, #19351, .T. ) ;
#3335 = AXIS2_PLACEMENT_3D ( 'NONE', #21027, #10856, #12194 ) ;
#3336 = FACE_OUTER_BOUND ( 'NONE', #7486, .T. ) ;
#3337 = DIRECTION ( 'NONE',  ( -1.000000000000000000, 0.000000000000000000, -0.000000000000000000 ) ) ;
#3338 = DIRECTION ( 'NONE',  ( -1.000000000000000000, 0.000000000000000000, 0.000000000000000000 ) ) ;
#3339 = CARTESIAN_POINT ( 'NONE',  ( 0.000000000000000000, 0.000000000000000000, 3.000000000000000000 ) ) ;
#3340 = PRODUCT_DEFINITION ( 'UNKNOWN', '', #3241, #15569 ) ;
#3341 = CARTESIAN_POINT ( 'NONE',  ( 5.000000000000002665, 23.62010150527335028, -84.77081340225880979 ) ) ;
#3342 = FACE_OUTER_BOUND ( 'NONE', #504, .T. ) ;
#3343 = CARTESIAN_POINT ( 'NONE',  ( 5.000000000000000000, 78.80192417387927151, 39.16958956249325752 ) ) ;
#3344 = CIRCLE ( 'NONE', #17808, 45.00000000000000000 ) ;
#3345 = VECTOR ( 'NONE', #18229, 1000.000000000000000 ) ;
#3346 = ORIENTED_EDGE ( 'NONE', *, *, #3253, .T. ) ;
#3347 = CIRCLE ( 'NONE', #9034, 44.99999999999999289 ) ;
#3348 = AXIS2_PLACEMENT_3D ( 'NONE', #17343, #20645, #13278 ) ;
#3349 = CARTESIAN_POINT ( 'NONE',  ( 5.000000000000000000, -61.60362715319078575, 62.84101464466223774 ) ) ;
#3350 = CARTESIAN_POINT ( 'NONE',  ( 0.000000000000000000, -15.51843147776295950, -83.63233659819665888 ) ) ;
#3351 = VERTEX_POINT ( 'NONE', #9070 ) ;
#3352 = CARTESIAN_POINT ( 'NONE',  ( 9.999999999999994671, 118.9000000000000199, 0.000000000000000000 ) ) ;
#3353 = VERTEX_POINT ( 'NONE', #5999 ) ;
#3354 = ORIENTED_EDGE ( 'NONE', *, *, #9862, .F. ) ;
#3355 = DIRECTION ( 'NONE',  ( 0.000000000000000000, 0.000000000000000000, -1.000000000000000000 ) ) ;
#3356 = EDGE_LOOP ( 'NONE', ( #14008, #18777, #18066, #17907 ) ) ;
#3357 = ADVANCED_FACE ( 'NONE', ( #5767 ), #4110, .F. ) ;
#3358 = CIRCLE ( 'NONE', #3016, 44.99999999999999289 ) ;
#3359 = AXIS2_PLACEMENT_3D ( 'NONE', #15552, #18666, #417 ) ;
#3360 = ORIENTED_EDGE ( 'NONE', *, *, #21249, .T. ) ;
#3361 = CARTESIAN_POINT ( 'NONE',  ( 0.000000000000000000, 5.000000000000004441, 0.000000000000000000 ) ) ;
#3362 = DIRECTION ( 'NONE',  ( 0.000000000000000000, -0.8290375725550469532, 0.5591929034707392443 ) ) ;
#3363 = AXIS2_PLACEMENT_3D ( 'NONE', #9186, #4227, #12723 ) ;
#3364 = ORIENTED_EDGE ( 'NONE', *, *, #14710, .T. ) ;
#3365 = CIRCLE ( 'NONE', #2645, 44.99999999999998579 ) ;
#3366 = CIRCLE ( 'NONE', #10408, 27.49900000000000588 ) ;
#3367 = DIRECTION ( 'NONE',  ( -1.000000000000000000, 0.000000000000000000, 0.000000000000000000 ) ) ;
#3368 = CARTESIAN_POINT ( 'NONE',  ( 0.000000000000000000, 0.000000000000000000, 0.000000000000000000 ) ) ;
#3369 = DIRECTION ( 'NONE',  ( -1.000000000000000000, 0.000000000000000000, 0.000000000000000000 ) ) ;
#3370 = CARTESIAN_POINT ( 'NONE',  ( 10.00000000000000000, 51.10509369859433804, 77.10190917907216601 ) ) ;
#3371 = DIRECTION ( 'NONE',  ( 0.000000000000000000, 0.000000000000000000, 1.000000000000000000 ) ) ;
#3372 = CARTESIAN_POINT ( 'NONE',  ( 5.000000000000000888, 7.240962358591573889, 31.16999300804317130 ) ) ;
#3373 = AXIS2_PLACEMENT_3D ( 'NONE', #14640, #14859, #4810 ) ;
#3374 = EDGE_LOOP ( 'NONE', ( #8969, #10841, #7132, #19223, #12207, #12919, #20490, #3421, #2793, #6559, #6553, #20813, #11033, #69, #10042, #2692, #3039, #15723, #15870, #18021, #6426, #4324, #6587, #266, #3745, #1261, #7596, #15067, #4578, #1410, #13434, #2511, #17413, #5644, #21082, #16794, #18903, #6060, #1391, #19828, #17230, #20859, #15015, #13319, #17120, #4446, #14159, #2430, #10280, #16279, #11122, #13524, #5559, #6472, #19722, #1160, #13205, #10003, #21548, #10058, #3594, #5403, #14502, #11179, #1941, #15392, #17303, #2529, #5193, #5236, #11106, #9376, #20906, #9254, #1815, #5324, #11722, #17087, #5885, #14492, #19873, #17446, #13870, #17770, #4353, #3009, #14165, #8364, #4855, #13484, #14296, #9483, #582, #6312, #11857, #186, #13485, #12726, #9145, #15041, #296, #2467, #11132, #11068, #5102, #5625, #3001, #13030, #18015, #12537, #15363, #5164, #4334, #12638, #18939, #15842, #11091, #8196, #12231, #3879, #2531, #8498, #13919, #7541, #12816 ) ) ;
#3375 = CARTESIAN_POINT ( 'NONE',  ( 0.000000000000000000, -22.77465461094663368, -15.41136296218110147 ) ) ;
#3376 = EDGE_CURVE ( 'NONE', #17660, #12864, #1317, .T. ) ;
#3377 = CYLINDRICAL_SURFACE ( 'NONE', #4800, 3.000000000000000000 ) ;
#3378 = EDGE_LOOP ( 'NONE', ( #7901, #14842, #51, #18970 ) ) ;
#3379 = VECTOR ( 'NONE', #12607, 1000.000000000000000 ) ;
#3380 = CIRCLE ( 'NONE', #5157, 27.49900000000000233 ) ;
#3381 = EDGE_CURVE ( 'NONE', #2483, #1347, #943, .T. ) ;
#3382 = DIRECTION ( 'NONE',  ( 0.000000000000000000, -0.9848077530122062440, -0.1736481776669404620 ) ) ;
#3383 = AXIS2_PLACEMENT_3D ( 'NONE', #12489, #19033, #3889 ) ;
#3384 = ORIENTED_EDGE ( 'NONE', *, *, #9576, .F. ) ;
#3385 = DIRECTION ( 'NONE',  ( 0.000000000000000000, -0.2079116908177468248, -0.9781476007338083534 ) ) ;
#3386 = CARTESIAN_POINT ( 'NONE',  ( 10.00000000000000000, 0.000000000000000000, 0.000000000000000000 ) ) ;
#3387 = VERTEX_POINT ( 'NONE', #15922 ) ;
#3388 = DIRECTION ( 'NONE',  ( -1.000000000000000000, -0.000000000000000000, -0.000000000000000000 ) ) ;
#3390 = EDGE_CURVE ( 'NONE', #2869, #13770, #2709, .T. ) ;
#3389 = ORIENTED_EDGE ( 'NONE', *, *, #12322, .F. ) ;
#3391 = EDGE_LOOP ( 'NONE', ( #7631, #17168 ) ) ;
#3392 = EDGE_CURVE ( 'NONE', #16153, #2852, #4873, .T. ) ;
#3393 = ORIENTED_EDGE ( 'NONE', *, *, #15717, .T. ) ;
#3394 = EDGE_CURVE ( 'NONE', #12590, #9562, #7647, .T. ) ;
#3395 = DIRECTION ( 'NONE',  ( 0.000000000000000000, 0.000000000000000000, 1.000000000000000000 ) ) ;
#3396 = ORIENTED_EDGE ( 'NONE', *, *, #1122, .T. ) ;
#3397 = DIRECTION ( 'NONE',  ( -1.000000000000000000, 0.000000000000000000, -0.000000000000000000 ) ) ;
#3398 = EDGE_CURVE ( 'NONE', #15174, #1347, #16682, .T. ) ;
#3399 = DIRECTION ( 'NONE',  ( 0.000000000000000000, 0.5877852522924741363, -0.8090169943749466741 ) ) ;
#3400 = CARTESIAN_POINT ( 'NONE',  ( 0.000000000000000000, 51.10509369859540385, -77.10190917907144126 ) ) ;
#3401 = CIRCLE ( 'NONE', #6231, 5.000000000000000000 ) ;
#3402 = DIRECTION ( 'NONE',  ( 1.000000000000000000, 0.000000000000000000, 0.000000000000000000 ) ) ;
#3403 = CARTESIAN_POINT ( 'NONE',  ( 10.00000000000000000, 57.06999622551805373, 66.98518889142101784 ) ) ;
#3404 = AXIS2_PLACEMENT_3D ( 'NONE', #21359, #19703, #14616 ) ;
#3405 = AXIS2_PLACEMENT_3D ( 'NONE', #7930, #19756, #14784 ) ;
#3406 = DIRECTION ( 'NONE',  ( 1.000000000000000000, -0.000000000000000000, -0.000000000000000000 ) ) ;
#3407 = DIRECTION ( 'NONE',  ( -1.000000000000000000, -0.000000000000000000, -0.000000000000000000 ) ) ;
#3408 = DIRECTION ( 'NONE',  ( 0.000000000000000000, 0.000000000000000000, 1.000000000000000000 ) ) ;
#3409 = EDGE_CURVE ( 'NONE', #16206, #4982, #19893, .T. ) ;
#3410 = CARTESIAN_POINT ( 'NONE',  ( 5.000000000000000000, -27.40684453873977944, 16.51862198942000148 ) ) ;
#3411 = EDGE_CURVE ( 'NONE', #6130, #3216, #7852, .T. ) ;
#3412 = CARTESIAN_POINT ( 'NONE',  ( 0.000000000000000000, 3.974475837764924968, 92.41557521768191918 ) ) ;
#3413 = EDGE_LOOP ( 'NONE', ( #10496, #1416, #20055, #4198 ) ) ;
#3414 = VECTOR ( 'NONE', #6743, 1000.000000000000000 ) ;
#3415 = ORIENTED_EDGE ( 'NONE', *, *, #331, .T. ) ;
#3416 = CARTESIAN_POINT ( 'NONE',  ( 10.00000000000000000, -74.39348546125016526, -54.97312363261490731 ) ) ;
#3417 = VECTOR ( 'NONE', #19348, 1000.000000000000000 ) ;
#3418 = EDGE_CURVE ( 'NONE', #15453, #16302, #21057, .T. ) ;
#3419 = ORIENTED_EDGE ( 'NONE', *, *, #12687, .T. ) ;
#3420 = VERTEX_POINT ( 'NONE', #15029 ) ;
#3421 = ORIENTED_EDGE ( 'NONE', *, *, #16613, .F. ) ;
#3422 = CARTESIAN_POINT ( 'NONE',  ( -90.00000000000000000, 0.000000000000000000, 0.000000000000000000 ) ) ;
#3423 = EDGE_CURVE ( 'NONE', #19711, #18608, #11612, .T. ) ;
#3424 = VERTEX_POINT ( 'NONE', #13369 ) ;
#3425 = FACE_OUTER_BOUND ( 'NONE', #8342, .T. ) ;
#3426 = CARTESIAN_POINT ( 'NONE',  ( -10.00000000000002309, 1.393954219129474843E-14, 113.8250000000000028 ) ) ;
#3427 = AXIS2_PLACEMENT_3D ( 'NONE', #10166, #13471, #6978 ) ;
#3428 = FACE_OUTER_BOUND ( 'NONE', #17603, .T. ) ;
#3429 = AXIS2_PLACEMENT_3D ( 'NONE', #2838, #19303, #20958 ) ;
#3430 = CARTESIAN_POINT ( 'NONE',  ( 5.000000000000002665, -46.07110168784768689, -74.97635353408431058 ) ) ;
#3431 = CARTESIAN_POINT ( 'NONE',  ( 10.00000000000000000, -31.15801000616779248, -79.14775961996421927 ) ) ;
#3432 = VECTOR ( 'NONE', #7502, 1000.000000000000000 ) ;
#3433 = CARTESIAN_POINT ( 'NONE',  ( 10.00000000000000000, 84.33453774737672859, -11.08490790852044405 ) ) ;
#3434 = CYLINDRICAL_SURFACE ( 'NONE', #2785, 92.50100000000000477 ) ;
#3435 = ORIENTED_EDGE ( 'NONE', *, *, #3394, .T. ) ;
#3436 = ADVANCED_FACE ( 'NONE', ( #18364 ), #12929, .F. ) ;
#3437 = DIRECTION ( 'NONE',  ( 0.000000000000000000, -0.1391731009600517543, -0.9902680687415721383 ) ) ;
#3438 = EDGE_LOOP ( 'NONE', ( #12551, #6391, #3602, #14766 ) ) ;
#3439 = EDGE_CURVE ( 'NONE', #3621, #16306, #6434, .T. ) ;
#3440 = VERTEX_POINT ( 'NONE', #20123 ) ;
#3441 = CIRCLE ( 'NONE', #960, 92.50099999999999056 ) ;
#3442 = DIRECTION ( 'NONE',  ( 0.000000000000000000, 0.000000000000000000, 1.000000000000000000 ) ) ;
#3443 = ORIENTED_EDGE ( 'NONE', *, *, #17842, .T. ) ;
#3444 = AXIS2_PLACEMENT_3D ( 'NONE', #13651, #20402, #10650 ) ;
#3445 = DIRECTION ( 'NONE',  ( -1.000000000000000000, -0.000000000000000000, -0.000000000000000000 ) ) ;
#3446 = ORIENTED_EDGE ( 'NONE', *, *, #15120, .F. ) ;
#3447 = ORIENTED_EDGE ( 'NONE', *, *, #2961, .F. ) ;
#3448 = AXIS2_PLACEMENT_3D ( 'NONE', #16884, #18441, #5386 ) ;
#3449 = ITEM_DEFINED_TRANSFORMATION ( 'NONE', 'NONE', #413,  #15567 ) ;
#3450 = CARTESIAN_POINT ( 'NONE',  ( -90.00000000000000000, 0.000000000000000000, 0.000000000000000000 ) ) ;
#3451 = ORIENTED_EDGE ( 'NONE', *, *, #20161, .T. ) ;
#3452 = CARTESIAN_POINT ( 'NONE',  ( 10.00000000000000000, 74.74361964203228581, 40.60271866773572214 ) ) ;
#3453 = CARTESIAN_POINT ( 'NONE',  ( 9.999999999999994671, 101.1000000000000512, 0.000000000000000000 ) ) ;
#3454 = DIRECTION ( 'NONE',  ( -1.000000000000000000, -0.000000000000000000, -0.000000000000000000 ) ) ;
#3455 = CARTESIAN_POINT ( 'NONE',  ( 0.000000000000000000, 0.000000000000000000, 100.0000000000000000 ) ) ;
#3456 = CARTESIAN_POINT ( 'NONE',  ( 0.000000000000000000, 28.15804365424197186, -1.358152127006073684 ) ) ;
#3457 = CARTESIAN_POINT ( 'NONE',  ( 10.00000000000000000, -23.10190250628894404, 89.56973317806591695 ) ) ;
#3458 = CYLINDRICAL_SURFACE ( 'NONE', #7724, 32.00000000000000000 ) ;
#3459 = AXIS2_PLACEMENT_3D ( 'NONE', #8314, #21785, #14829 ) ;
#3460 = CIRCLE ( 'NONE', #21448, 123.5000000000000142 ) ;
#3461 = AXIS2_PLACEMENT_3D ( 'NONE', #19402, #1167, #7908 ) ;
#3462 = ORIENTED_EDGE ( 'NONE', *, *, #11942, .T. ) ;
#3463 = AXIS2_PLACEMENT_3D ( 'NONE', #4576, #20150, #6245 ) ;
#3464 = CYLINDRICAL_SURFACE ( 'NONE', #4166, 123.5000000000000142 ) ;
#3465 = CARTESIAN_POINT ( 'NONE',  ( 10.00000000000000000, 23.62010150527335028, -84.77081340225880979 ) ) ;
#3466 = VERTEX_POINT ( 'NONE', #16583 ) ;
#3467 = CARTESIAN_POINT ( 'NONE',  ( 10.00000000000000000, -9.646732466564730046, -84.51112348751858860 ) ) ;
#3468 = ORIENTED_EDGE ( 'NONE', *, *, #18425, .F. ) ;
#3469 =( NAMED_UNIT ( * ) SI_UNIT ( $, .STERADIAN. ) SOLID_ANGLE_UNIT ( ) );
#3470 = CIRCLE ( 'NONE', #1359, 88.00000000000000000 ) ;
#3471 = EDGE_LOOP ( 'NONE', ( #21241, #8326, #18674, #13746 ) ) ;
#3472 = DIRECTION ( 'NONE',  ( 1.000000000000000000, 0.000000000000000000, 0.000000000000000000 ) ) ;
#3473 = VERTEX_POINT ( 'NONE', #6328 ) ;
#3474 = ORIENTED_EDGE ( 'NONE', *, *, #6090, .F. ) ;
#3475 = CARTESIAN_POINT ( 'NONE',  ( 10.00000000000000000, 0.000000000000000000, 0.000000000000000000 ) ) ;
#3476 = AXIS2_PLACEMENT_3D ( 'NONE', #13054, #13384, #21670 ) ;
#3477 = DIRECTION ( 'NONE',  ( 0.000000000000000000, 0.000000000000000000, 1.000000000000000000 ) ) ;
#3478 = AXIS2_PLACEMENT_3D ( 'NONE', #7429, #14259, #15822 ) ;
#3479 = VERTEX_POINT ( 'NONE', #21657 ) ;
#3480 = FACE_OUTER_BOUND ( 'NONE', #17737, .T. ) ;
#3481 = DIRECTION ( 'NONE',  ( 0.000000000000000000, 0.000000000000000000, -1.000000000000000000 ) ) ;
#3482 = DIRECTION ( 'NONE',  ( 0.000000000000000000, 0.000000000000000000, 1.000000000000000000 ) ) ;
#3483 = CARTESIAN_POINT ( 'NONE',  ( -1.500000000000001332, 0.000000000000000000, -7.400000000000019895 ) ) ;
#3484 = CARTESIAN_POINT ( 'NONE',  ( -1.399999999999998579, 0.000000000000000000, 0.000000000000000000 ) ) ;
#3485 = FACE_OUTER_BOUND ( 'NONE', #20052, .T. ) ;
#3486 = VERTEX_POINT ( 'NONE', #6210 ) ;
#3487 = DIRECTION ( 'NONE',  ( -1.000000000000000000, -0.000000000000000000, 0.000000000000000000 ) ) ;
#3488 = AXIS2_PLACEMENT_3D ( 'NONE', #7718, #11140, #17889 ) ;
#3489 = CARTESIAN_POINT ( 'NONE',  ( 10.00000000000000000, 0.000000000000000000, 0.000000000000000000 ) ) ;
#3490 = ADVANCED_FACE ( 'NONE', ( #9939 ), #4545, .F. ) ;
#3491 = AXIS2_PLACEMENT_3D ( 'NONE', #9136, #15889, #7489 ) ;
#3492 = ORIENTED_EDGE ( 'NONE', *, *, #12062, .T. ) ;
#3493 = AXIS2_PLACEMENT_3D ( 'NONE', #18206, #11010, #5945 ) ;
#3494 = DIRECTION ( 'NONE',  ( 0.000000000000000000, 0.000000000000000000, -1.000000000000000000 ) ) ;
#3495 = ORIENTED_EDGE ( 'NONE', *, *, #21273, .T. ) ;
#3496 = CARTESIAN_POINT ( 'NONE',  ( 10.00000000000000000, 0.000000000000000000, 0.000000000000000000 ) ) ;
#3497 = DIRECTION ( 'NONE',  ( 0.000000000000000000, 0.000000000000000000, -1.000000000000000000 ) ) ;
#3498 = ORIENTED_EDGE ( 'NONE', *, *, #6387, .F. ) ;
#3499 = EDGE_CURVE ( 'NONE', #9108, #13997, #4485, .T. ) ;
#3500 = DIRECTION ( 'NONE',  ( 1.000000000000000000, 0.000000000000000000, 0.000000000000000000 ) ) ;
#3501 = ORIENTED_EDGE ( 'NONE', *, *, #16648, .T. ) ;
#3502 = ORIENTED_EDGE ( 'NONE', *, *, #10695, .F. ) ;
#3503 = DIRECTION ( 'NONE',  ( -1.000000000000000000, -0.000000000000000000, 0.000000000000000000 ) ) ;
#3504 = ORIENTED_EDGE ( 'NONE', *, *, #2335, .T. ) ;
#3505 = EDGE_CURVE ( 'NONE', #12778, #11100, #19788, .T. ) ;
#3506 = DIRECTION ( 'NONE',  ( -1.000000000000000000, -0.000000000000000000, -0.000000000000000000 ) ) ;
#3507 = VECTOR ( 'NONE', #13222, 1000.000000000000000 ) ;
#3508 = CYLINDRICAL_SURFACE ( 'NONE', #7217, 92.50100000000000477 ) ;
#3509 = DIRECTION ( 'NONE',  ( -1.000000000000000000, 0.000000000000000000, -0.000000000000000000 ) ) ;
#3510 = CARTESIAN_POINT ( 'NONE',  ( 10.00000000000000000, 5.479102470011647519, -87.82926298292107958 ) ) ;
#3511 = CIRCLE ( 'NONE', #21510, 92.50100000000000477 ) ;
#3512 = AXIS2_PLACEMENT_3D ( 'NONE', #19768, #4630, #18108 ) ;
#3513 = DIRECTION ( 'NONE',  ( -1.000000000000000000, 0.000000000000000000, -0.000000000000000000 ) ) ;
#3514 = CYLINDRICAL_SURFACE ( 'NONE', #2733, 88.00000000000000000 ) ;
#3515 = CARTESIAN_POINT ( 'NONE',  ( 0.000000000000000000, 0.000000000000000000, 0.000000000000000000 ) ) ;
#3516 = DIRECTION ( 'NONE',  ( 0.000000000000000000, 0.000000000000000000, 1.000000000000000000 ) ) ;
#3517 = DIRECTION ( 'NONE',  ( 1.000000000000000000, 0.000000000000000000, 0.000000000000000000 ) ) ;
#3518 = EDGE_CURVE ( 'NONE', #16436, #15664, #16478, .T. ) ;
#3519 = ADVANCED_FACE ( 'NONE', ( #9715 ), #14816, .T. ) ;
#3520 = EDGE_CURVE ( 'NONE', #15608, #6772, #14354, .T. ) ;
#3521 = CARTESIAN_POINT ( 'NONE',  ( 0.000000000000000000, 0.000000000000000000, 0.000000000000000000 ) ) ;
#3522 = VERTEX_POINT ( 'NONE', #10052 ) ;
#3523 = EDGE_CURVE ( 'NONE', #5168, #14060, #12236, .T. ) ;
#3524 = CARTESIAN_POINT ( 'NONE',  ( -10.00000000000000000, 0.000000000000000000, 0.000000000000000000 ) ) ;
#3525 = VERTEX_POINT ( 'NONE', #16354 ) ;
#3526 = AXIS2_PLACEMENT_3D ( 'NONE', #3896, #14059, #10301 ) ;
#3527 = CARTESIAN_POINT ( 'NONE',  ( 0.000000000000000000, 0.000000000000000000, 0.000000000000000000 ) ) ;
#3528 = CIRCLE ( 'NONE', #6364, 88.00000000000000000 ) ;
#3529 = ORIENTED_EDGE ( 'NONE', *, *, #4313, .F. ) ;
#3530 = VERTEX_POINT ( 'NONE', #1226 ) ;
#3531 = ORIENTED_EDGE ( 'NONE', *, *, #19424, .T. ) ;
#3532 = EDGE_CURVE ( 'NONE', #9814, #16595, #16118, .T. ) ;
#3533 = CARTESIAN_POINT ( 'NONE',  ( 10.00000000000000000, -82.02147376274642454, -42.76579056660944644 ) ) ;
#3534 = ORIENTED_EDGE ( 'NONE', *, *, #7952, .F. ) ;
#3535 = DIRECTION ( 'NONE',  ( 0.000000000000000000, 0.000000000000000000, -1.000000000000000000 ) ) ;
#3536 = SURFACE_STYLE_FILL_AREA ( #18684 ) ;
#3537 = EDGE_CURVE ( 'NONE', #5209, #11505, #20372, .T. ) ;
#3538 = CYLINDRICAL_SURFACE ( 'NONE', #7512, 44.99999999999999289 ) ;
#3539 = PLANE ( 'NONE',  #9399 ) ;
#3540 = DIRECTION ( 'NONE',  ( -1.000000000000000000, -0.000000000000000000, -0.000000000000000000 ) ) ;
#3541 = VECTOR ( 'NONE', #4443, 1000.000000000000000 ) ;
#3542 = CARTESIAN_POINT ( 'NONE',  ( 10.00000000000000000, 27.26034713664097353, -7.182859710736244629 ) ) ;
#3543 = DIRECTION ( 'NONE',  ( 0.000000000000000000, 0.000000000000000000, 1.000000000000000000 ) ) ;
#3544 = VERTEX_POINT ( 'NONE', #13705 ) ;
#3545 = DIRECTION ( 'NONE',  ( 0.000000000000000000, -0.9993908270190959842, 0.03489949670249112984 ) ) ;
#3546 = ADVANCED_FACE ( 'NONE', ( #112 ), #2363, .T. ) ;
#3547 = ORIENTED_EDGE ( 'NONE', *, *, #18928, .T. ) ;
#3548 = ORIENTED_EDGE ( 'NONE', *, *, #10020, .F. ) ;
#3549 = DIRECTION ( 'NONE',  ( 0.000000000000000000, 0.000000000000000000, -1.000000000000000000 ) ) ;
#3550 = VERTEX_POINT ( 'NONE', #1668 ) ;
#3551 = CIRCLE ( 'NONE', #20497, 11.99999999999999822 ) ;
#3552 = CARTESIAN_POINT ( 'NONE',  ( 10.00000000000000000, -81.32027326007897727, 44.08455690949027428 ) ) ;
#3553 = VERTEX_POINT ( 'NONE', #15468 ) ;
#3554 = ORIENTED_EDGE ( 'NONE', *, *, #14704, .F. ) ;
#3555 = PRODUCT_CONTEXT ( 'NONE', #17866, 'mechanical' ) ;
#3556 = EDGE_CURVE ( 'NONE', #11575, #9822, #5317, .T. ) ;
#3557 = CARTESIAN_POINT ( 'NONE',  ( 0.000000000000000000, 87.44637528609661103, 9.855528870798920593 ) ) ;
#3558 = ORIENTED_EDGE ( 'NONE', *, *, #7628, .F. ) ;
#3559 = EDGE_CURVE ( 'NONE', #17337, #1046, #15403, .T. ) ;
#3560 = CARTESIAN_POINT ( 'NONE',  ( 10.00000000000000000, 87.58454185039441597, 8.540961822681984117 ) ) ;
#3561 = DIRECTION ( 'NONE',  ( -1.000000000000000000, -0.000000000000000000, 0.000000000000000000 ) ) ;
#3562 = CYLINDRICAL_SURFACE ( 'NONE', #11415, 44.99999999999999289 ) ;
#3563 = AXIS2_PLACEMENT_3D ( 'NONE', #18629, #16637, #4934 ) ;
#3564 = DIRECTION ( 'NONE',  ( -1.000000000000000000, 0.000000000000000000, 0.000000000000000000 ) ) ;
#3565 = EDGE_CURVE ( 'NONE', #4256, #19013, #6972, .T. ) ;
#3566 = EDGE_CURVE ( 'NONE', #17521, #12476, #11939, .T. ) ;
#3567 = CARTESIAN_POINT ( 'NONE',  ( 10.00000000000000000, -31.75612719289738095, -3.943144139962873940 ) ) ;
#3568 = DIRECTION ( 'NONE',  ( 0.000000000000000000, 0.000000000000000000, -1.000000000000000000 ) ) ;
#3569 = CARTESIAN_POINT ( 'NONE',  ( 0.000000000000000000, -6.063030049135288202, 31.42037024962122871 ) ) ;
#3570 = COLOUR_RGB ( '', 0.40784314, 0.44705882, 0.49803922) ;
#3571 = ORIENTED_EDGE ( 'NONE', *, *, #5967, .F. ) ;
#3572 = DIRECTION ( 'NONE',  ( 0.000000000000000000, 0.000000000000000000, 1.000000000000000000 ) ) ;
#3573 = CYLINDRICAL_SURFACE ( 'NONE', #17647, 44.99999999999998579 ) ;
#3574 = ORIENTED_EDGE ( 'NONE', *, *, #17274, .T. ) ;
#3575 = DIRECTION ( 'NONE',  ( 1.000000000000000000, -0.000000000000000000, -0.000000000000000000 ) ) ;
#3576 = ORIENTED_EDGE ( 'NONE', *, *, #21090, .T. ) ;
#3577 = ORIENTED_EDGE ( 'NONE', *, *, #4325, .F. ) ;
#3578 = DIRECTION ( 'NONE',  ( 0.000000000000000000, -0.8987940462991711454, 0.4383711467890689661 ) ) ;
#3579 = AXIS2_PLACEMENT_3D ( 'NONE', #13970, #921, #17513 ) ;
#3580 = ORIENTED_EDGE ( 'NONE', *, *, #133, .F. ) ;
#3581 = VERTEX_POINT ( 'NONE', #18690 ) ;
#3582 =( GEOMETRIC_REPRESENTATION_CONTEXT ( 3 ) GLOBAL_UNCERTAINTY_ASSIGNED_CONTEXT ( ( #3261 ) ) GLOBAL_UNIT_ASSIGNED_CONTEXT ( ( #9086, #375, #5457 ) ) REPRESENTATION_CONTEXT ( 'NONE', 'WORKASPACE' ) );
#3583 = DIRECTION ( 'NONE',  ( 0.000000000000000000, -0.7431448254773861395, -0.6691306063588670083 ) ) ;
#3584 = DIRECTION ( 'NONE',  ( 1.000000000000000000, 0.000000000000000000, 0.000000000000000000 ) ) ;
#3585 = CYLINDRICAL_SURFACE ( 'NONE', #13569, 113.8250000000000171 ) ;
#3586 = CARTESIAN_POINT ( 'NONE',  ( -10.49999999999999822, 0.000000000000000000, 3.000000000000000000 ) ) ;
#3587 = CARTESIAN_POINT ( 'NONE',  ( 10.00000000000000000, -37.96946988134224910, 76.11510229470846411 ) ) ;
#3588 = DIRECTION ( 'NONE',  ( 0.000000000000000000, 0.000000000000000000, -1.000000000000000000 ) ) ;
#3589 = DIRECTION ( 'NONE',  ( 0.000000000000000000, 0.4694715627858855322, 0.8829475928589297640 ) ) ;
#3590 = CARTESIAN_POINT ( 'NONE',  ( 10.00000000000000000, 0.000000000000000000, 0.000000000000000000 ) ) ;
#3591 = VERTEX_POINT ( 'NONE', #15236 ) ;
#3592 = FACE_OUTER_BOUND ( 'NONE', #449, .T. ) ;
#3593 = DIRECTION ( 'NONE',  ( 0.000000000000000000, 0.000000000000000000, 1.000000000000000000 ) ) ;
#3594 = ORIENTED_EDGE ( 'NONE', *, *, #12454, .F. ) ;
#3595 = DIRECTION ( 'NONE',  ( 1.000000000000000000, -0.000000000000000000, -0.000000000000000000 ) ) ;
#3596 = ORIENTED_EDGE ( 'NONE', *, *, #8557, .F. ) ;
#3597 = CARTESIAN_POINT ( 'NONE',  ( 10.00000000000000000, -79.66702613806754130, -29.80527447819517661 ) ) ;
#3598 = FACE_OUTER_BOUND ( 'NONE', #15071, .T. ) ;
#3599 = VERTEX_POINT ( 'NONE', #6759 ) ;
#3600 = ORIENTED_EDGE ( 'NONE', *, *, #10002, .F. ) ;
#3601 = ORIENTED_EDGE ( 'NONE', *, *, #11119, .F. ) ;
#3602 = ORIENTED_EDGE ( 'NONE', *, *, #7155, .F. ) ;
#3603 = FACE_BOUND ( 'NONE', #17109, .T. ) ;
#3604 = ORIENTED_EDGE ( 'NONE', *, *, #10789, .F. ) ;
#3605 = DIRECTION ( 'NONE',  ( -1.000000000000000000, 0.000000000000000000, -0.000000000000000000 ) ) ;
#3606 = FACE_OUTER_BOUND ( 'NONE', #14526, .T. ) ;
#3607 = DIRECTION ( 'NONE',  ( 0.000000000000000000, -0.2079116908177469081, -0.9781476007338083534 ) ) ;
#3608 = EDGE_CURVE ( 'NONE', #14246, #15239, #18788, .T. ) ;
#3609 = CARTESIAN_POINT ( 'NONE',  ( 10.00000000000000000, -3.728035544475628793, -84.97818067823773447 ) ) ;
#3610 = CARTESIAN_POINT ( 'NONE',  ( 10.00000000000000000, -67.05625154133410604, -63.71729851637880415 ) ) ;
#3611 = CARTESIAN_POINT ( 'NONE',  ( 10.00000000000000000, -90.32141448704669529, -19.96189084378313794 ) ) ;
#3612 = CARTESIAN_POINT ( 'NONE',  ( -8.900000000000019895, 1.231382356542664155E-14, 100.0000000000000284 ) ) ;
#3613 = CYLINDRICAL_SURFACE ( 'NONE', #1148, 44.99999999999999289 ) ;
#3614 = ORIENTED_EDGE ( 'NONE', *, *, #3297, .T. ) ;
#3615 = EDGE_CURVE ( 'NONE', #13385, #17227, #7311, .T. ) ;
#3616 = FACE_OUTER_BOUND ( 'NONE', #1282, .T. ) ;
#3617 = AXIS2_PLACEMENT_3D ( 'NONE', #15129, #1767, #11710 ) ;
#3618 = CARTESIAN_POINT ( 'NONE',  ( 10.00000000000000000, 86.66425444033919234, 32.33793443156426406 ) ) ;
#3619 = AXIS2_PLACEMENT_3D ( 'NONE', #15109, #3407, #16885 ) ;
#3620 = DIRECTION ( 'NONE',  ( 0.000000000000000000, 0.000000000000000000, -1.000000000000000000 ) ) ;
#3621 = VERTEX_POINT ( 'NONE', #229 ) ;
#3622 = CARTESIAN_POINT ( 'NONE',  ( 10.00000000000000000, -84.33453774737651543, -11.08490790852216534 ) ) ;
#3623 = ORIENTED_EDGE ( 'NONE', *, *, #20532, .F. ) ;
#3624 = DIRECTION ( 'NONE',  ( 1.000000000000000000, 0.000000000000000000, 0.000000000000000000 ) ) ;
#3625 = ORIENTED_EDGE ( 'NONE', *, *, #10450, .F. ) ;
#3626 = AXIS2_PLACEMENT_3D ( 'NONE', #13701, #15784, #10697 ) ;
#3627 = ORIENTED_EDGE ( 'NONE', *, *, #19984, .F. ) ;
#3628 = VERTEX_POINT ( 'NONE', #3754 ) ;
#3629 = CARTESIAN_POINT ( 'NONE',  ( -90.00000000000000000, 8.239576745513314221E-16, 6.728125000000023448 ) ) ;
#3630 = CIRCLE ( 'NONE', #8222, 88.00000000000000000 ) ;
#3631 = ORIENTED_EDGE ( 'NONE', *, *, #16907, .F. ) ;
#3632 = DIRECTION ( 'NONE',  ( 1.000000000000000000, 0.000000000000000000, 0.000000000000000000 ) ) ;
#3633 = CARTESIAN_POINT ( 'NONE',  ( 0.000000000000000000, 0.000000000000000000, 0.000000000000000000 ) ) ;
#3634 = EDGE_CURVE ( 'NONE', #19720, #11833, #10375, .T. ) ;
#3635 = ADVANCED_FACE ( 'NONE', ( #13 ), #5418, .F. ) ;
#3636 = VECTOR ( 'NONE', #14719, 1000.000000000000000 ) ;
#3637 = DIRECTION ( 'NONE',  ( 1.000000000000000000, 0.000000000000000000, 0.000000000000000000 ) ) ;
#3638 = CARTESIAN_POINT ( 'NONE',  ( 0.000000000000000000, -92.49798535263880694, 0.7467976319017535225 ) ) ;
#3639 = DIRECTION ( 'NONE',  ( -1.000000000000000000, -0.000000000000000000, -0.000000000000000000 ) ) ;
#3640 = DIRECTION ( 'NONE',  ( -1.000000000000000000, 0.000000000000000000, 0.000000000000000000 ) ) ;
#3641 = DIRECTION ( 'NONE',  ( 0.000000000000000000, 0.000000000000000000, 1.000000000000000000 ) ) ;
#3642 = AXIS2_PLACEMENT_3D ( 'NONE', #6737, #4626, #6623 ) ;
#3643 = EDGE_LOOP ( 'NONE', ( #20257, #12651, #11816, #19041 ) ) ;
#3644 = CARTESIAN_POINT ( 'NONE',  ( 10.00000000000000000, -35.34277389771474986, -85.48288328206420772 ) ) ;
#3645 = EDGE_CURVE ( 'NONE', #2453, #10528, #255, .T. ) ;
#3646 = AXIS2_PLACEMENT_3D ( 'NONE', #5472, #169, #18628 ) ;
#3647 = ORIENTED_EDGE ( 'NONE', *, *, #21065, .F. ) ;
#3648 = VECTOR ( 'NONE', #1130, 1000.000000000000000 ) ;
#3649 = EDGE_LOOP ( 'NONE', ( #12915, #6031, #12301, #821 ) ) ;
#3650 = EDGE_CURVE ( 'NONE', #8089, #2646, #10827, .T. ) ;
#3651 = DIRECTION ( 'NONE',  ( 1.000000000000000000, 0.000000000000000000, 0.000000000000000000 ) ) ;
#3652 = ORIENTED_EDGE ( 'NONE', *, *, #5534, .T. ) ;
#3653 = ORIENTED_EDGE ( 'NONE', *, *, #11912, .F. ) ;
#3654 = DIRECTION ( 'NONE',  ( 1.000000000000000000, 0.000000000000000000, 0.000000000000000000 ) ) ;
#3655 = AXIS2_PLACEMENT_3D ( 'NONE', #7264, #15644, #20424 ) ;
#3656 = EDGE_CURVE ( 'NONE', #21588, #2240, #21421, .T. ) ;
#3657 = VERTEX_POINT ( 'NONE', #13912 ) ;
#3658 = ADVANCED_FACE ( 'NONE', ( #5523 ), #12255, .T. ) ;
#3659 = ADVANCED_FACE ( 'NONE', ( #11826 ), #18578, .F. ) ;
#3660 = DIRECTION ( 'NONE',  ( 1.000000000000000000, 0.000000000000000000, 0.000000000000000000 ) ) ;
#3661 = CIRCLE ( 'NONE', #5437, 11.99999999999999822 ) ;
#3662 = ADVANCED_FACE ( 'NONE', ( #10811 ), #15791, .F. ) ;
#3663 = CARTESIAN_POINT ( 'NONE',  ( 10.00000000000000000, -92.32475887865419395, -5.707354816231494432 ) ) ;
#3664 = CARTESIAN_POINT ( 'NONE',  ( -10.00000000000000000, 0.000000000000000000, 0.000000000000000000 ) ) ;
#3665 = DIRECTION ( 'NONE',  ( -1.000000000000000000, 0.000000000000000000, 0.000000000000000000 ) ) ;
#3666 = AXIS2_PLACEMENT_3D ( 'NONE', #9119, #15754, #21053 ) ;
#3667 = DIRECTION ( 'NONE',  ( 0.000000000000000000, 0.4067366430758008744, -0.9135454576426006446 ) ) ;
#3668 = DIRECTION ( 'NONE',  ( 1.000000000000000000, 0.000000000000000000, 0.000000000000000000 ) ) ;
#3669 = CARTESIAN_POINT ( 'NONE',  ( 10.00000000000000000, 0.000000000000000000, 0.000000000000000000 ) ) ;
#3670 = EDGE_LOOP ( 'NONE', ( #9750, #16754, #6405, #15038, #9979 ) ) ;
#3671 = EDGE_CURVE ( 'NONE', #6675, #9108, #2311, .T. ) ;
#3672 = AXIS2_PLACEMENT_3D ( 'NONE', #19832, #19733, #3048 ) ;
#3673 = EDGE_CURVE ( 'NONE', #10178, #21331, #18965, .T. ) ;
#3674 = CARTESIAN_POINT ( 'NONE',  ( 0.000000000000000000, 78.83848282823907994, 48.38314403117527718 ) ) ;
#3675 = CIRCLE ( 'NONE', #10377, 44.99999999999999289 ) ;
#3676 = DIRECTION ( 'NONE',  ( -1.000000000000000000, -0.000000000000000000, 0.000000000000000000 ) ) ;
#3677 = EDGE_LOOP ( 'NONE', ( #18265, #3534, #11480, #2970 ) ) ;
#3678 = CARTESIAN_POINT ( 'NONE',  ( 1.129531546211711479, 0.000000000000000000, 0.000000000000000000 ) ) ;
#3679 = ORIENTED_EDGE ( 'NONE', *, *, #16912, .F. ) ;
#3680 = CIRCLE ( 'NONE', #15683, 92.50100000000000477 ) ;
#3681 = EDGE_CURVE ( 'NONE', #419, #14686, #7505, .T. ) ;
#3682 = VERTEX_POINT ( 'NONE', #16116 ) ;
#3683 = CARTESIAN_POINT ( 'NONE',  ( 10.00000000000000000, 0.000000000000000000, 0.000000000000000000 ) ) ;
#3684 = EDGE_LOOP ( 'NONE', ( #21184, #12645, #131, #12882 ) ) ;
#3685 = ORIENTED_EDGE ( 'NONE', *, *, #11267, .F. ) ;
#3686 = CARTESIAN_POINT ( 'NONE',  ( 0.000000000000000000, 60.00000000000000000, -15.00000000000000000 ) ) ;
#3687 = FACE_OUTER_BOUND ( 'NONE', #8467, .T. ) ;
#3688 = CIRCLE ( 'NONE', #15690, 92.50100000000001899 ) ;
#3689 = EDGE_CURVE ( 'NONE', #15117, #3028, #17909, .T. ) ;
#3690 = CARTESIAN_POINT ( 'NONE',  ( 1.400000000000000133, 0.000000000000000000, 0.000000000000000000 ) ) ;
#3691 = LINE ( 'NONE', #10538, #9094 ) ;
#3692 = CIRCLE ( 'NONE', #14263, 45.00000000000000711 ) ;
#3693 = CARTESIAN_POINT ( 'NONE',  ( 0.000000000000000000, -32.56745702629792305, 78.57830605990643846 ) ) ;
#3694 = AXIS2_PLACEMENT_3D ( 'NONE', #19034, #11854, #5227 ) ;
#3695 = DIRECTION ( 'NONE',  ( 0.000000000000000000, 0.000000000000000000, 1.000000000000000000 ) ) ;
#3696 = CARTESIAN_POINT ( 'NONE',  ( 5.000000000000000000, -69.74988376403980794, -53.65588238863408321 ) ) ;
#3697 = DIRECTION ( 'NONE',  ( -1.000000000000000000, 0.000000000000000000, 0.000000000000000000 ) ) ;
#3698 = ORIENTED_EDGE ( 'NONE', *, *, #16892, .T. ) ;
#3699 = DIRECTION ( 'NONE',  ( -1.000000000000000000, 0.000000000000000000, 0.000000000000000000 ) ) ;
#3700 = EDGE_LOOP ( 'NONE', ( #4972, #4505, #15095, #8829 ) ) ;
#3701 = EDGE_CURVE ( 'NONE', #15534, #12050, #5857, .T. ) ;
#3702 = DIRECTION ( 'NONE',  ( 0.000000000000000000, -0.9702957262759939194, -0.2419218955996776110 ) ) ;
#3703 = ORIENTED_EDGE ( 'NONE', *, *, #14153, .T. ) ;
#3704 = VECTOR ( 'NONE', #9367, 1000.000000000000000 ) ;
#3705 = CARTESIAN_POINT ( 'NONE',  ( 0.000000000000000000, -78.83848282823873888, -48.38314403117582430 ) ) ;
#3706 = CIRCLE ( 'NONE', #8302, 45.00000000000000000 ) ;
#3707 = DIRECTION ( 'NONE',  ( 1.000000000000000000, 0.000000000000000000, 0.000000000000000000 ) ) ;
#3708 = VERTEX_POINT ( 'NONE', #5637 ) ;
#3709 = AXIS2_PLACEMENT_3D ( 'NONE', #13670, #198, #12226 ) ;
#3710 = EDGE_CURVE ( 'NONE', #14716, #935, #14237, .T. ) ;
#3711 =( NAMED_UNIT ( * ) PLANE_ANGLE_UNIT ( ) SI_UNIT ( $, .RADIAN. ) );
#3712 = CIRCLE ( 'NONE', #9343, 92.50100000000000477 ) ;
#3713 = ORIENTED_EDGE ( 'NONE', *, *, #4161, .F. ) ;
#3714 = ORIENTED_EDGE ( 'NONE', *, *, #11129, .T. ) ;
#3715 = ORIENTED_EDGE ( 'NONE', *, *, #13855, .F. ) ;
#3716 = CARTESIAN_POINT ( 'NONE',  ( 10.00000000000000000, 28.15804365424195765, 1.358152127006451826 ) ) ;
#3717 = AXIS2_PLACEMENT_3D ( 'NONE', #8373, #10456, #16986 ) ;
#3718 = ORIENTED_EDGE ( 'NONE', *, *, #11950, .T. ) ;
#3719 = FACE_OUTER_BOUND ( 'NONE', #8769, .T. ) ;
#3720 = CARTESIAN_POINT ( 'NONE',  ( 10.00000000000000000, -81.55207211302061410, -24.17537951050148592 ) ) ;
#3721 = DIRECTION ( 'NONE',  ( 1.000000000000000000, -0.000000000000000000, 0.000000000000000000 ) ) ;
#3722 = FACE_OUTER_BOUND ( 'NONE', #2898, .T. ) ;
#3723 = VECTOR ( 'NONE', #6474, 1000.000000000000000 ) ;
#3724 = CARTESIAN_POINT ( 'NONE',  ( 10.00000000000000000, -41.87002153499162915, 74.04114219178029543 ) ) ;
#3725 = CARTESIAN_POINT ( 'NONE',  ( -7.500000000000000000, 0.000000000000000000, 3.000000000000000000 ) ) ;
#3726 = CYLINDRICAL_SURFACE ( 'NONE', #7671, 11.99999999999999822 ) ;
#3727 = AXIS2_PLACEMENT_3D ( 'NONE', #2786, #17807, #2885 ) ;
#3728 = FACE_OUTER_BOUND ( 'NONE', #5127, .T. ) ;
#3729 = CIRCLE ( 'NONE', #543, 92.50099999999999056 ) ;
#3730 = VERTEX_POINT ( 'NONE', #20985 ) ;
#3731 = AXIS2_PLACEMENT_3D ( 'NONE', #3047, #13311, #21392 ) ;
#3732 = CYLINDRICAL_SURFACE ( 'NONE', #19740, 44.99999999999998579 ) ;
#3733 = VECTOR ( 'NONE', #7493, 1000.000000000000000 ) ;
#3734 = DIRECTION ( 'NONE',  ( 1.000000000000000000, 0.000000000000000000, 0.000000000000000000 ) ) ;
#3735 = ADVANCED_FACE ( 'NONE', ( #2635 ), #7669, .T. ) ;
#3736 = DIRECTION ( 'NONE',  ( -1.000000000000000000, -0.000000000000000000, -0.000000000000000000 ) ) ;
#3737 = ORIENTED_EDGE ( 'NONE', *, *, #17458, .F. ) ;
#3738 = CARTESIAN_POINT ( 'NONE',  ( 0.000000000000000000, 35.18804927320529430, 80.65854690202691302 ) ) ;
#3739 = ORIENTED_EDGE ( 'NONE', *, *, #21717, .T. ) ;
#3740 = DIRECTION ( 'NONE',  ( 0.000000000000000000, 0.000000000000000000, 1.000000000000000000 ) ) ;
#3741 = EDGE_LOOP ( 'NONE', ( #19875, #14357, #8100, #6667 ) ) ;
#3742 = ORIENTED_EDGE ( 'NONE', *, *, #13016, .F. ) ;
#3743 = AXIS2_PLACEMENT_3D ( 'NONE', #6438, #1448, #1780 ) ;
#3744 = CIRCLE ( 'NONE', #11153, 88.00000000000000000 ) ;
#3745 = ORIENTED_EDGE ( 'NONE', *, *, #2425, .F. ) ;
#3746 = CIRCLE ( 'NONE', #6895, 92.50100000000003320 ) ;
#3747 = DIRECTION ( 'NONE',  ( 0.000000000000000000, 0.000000000000000000, 1.000000000000000000 ) ) ;
#3748 = DIRECTION ( 'NONE',  ( 1.000000000000000000, 0.000000000000000000, 0.000000000000000000 ) ) ;
#3749 = CARTESIAN_POINT ( 'NONE',  ( 10.00000000000000000, -92.49798535263880694, 0.7467976319017460840 ) ) ;
#3750 = CARTESIAN_POINT ( 'NONE',  ( 0.000000000000000000, 64.95266917914399585, -59.37298010462904330 ) ) ;
#3751 = DIRECTION ( 'NONE',  ( -1.000000000000000000, 0.000000000000000000, 0.000000000000000000 ) ) ;
#3752 = DIRECTION ( 'NONE',  ( 1.000000000000000000, 0.000000000000000000, -0.000000000000000000 ) ) ;
#3753 = DIRECTION ( 'NONE',  ( 0.000000000000000000, -0.5877852522924797984, 0.8090169943749426773 ) ) ;
#3754 = CARTESIAN_POINT ( 'NONE',  ( 10.00000000000000000, -21.69483248597410707, -16.89761061231802586 ) ) ;
#3755 = DIRECTION ( 'NONE',  ( -1.000000000000000000, 0.000000000000000000, -0.000000000000000000 ) ) ;
#3756 = AXIS2_PLACEMENT_3D ( 'NONE', #5971, #17784, #9370 ) ;
#3757 = ORIENTED_EDGE ( 'NONE', *, *, #7331, .T. ) ;
#3758 = CIRCLE ( 'NONE', #17537, 5.000000000000000000 ) ;
#3759 = CARTESIAN_POINT ( 'NONE',  ( 0.000000000000000000, 46.07110168784820559, 74.97635353408399794 ) ) ;
#3760 = EDGE_LOOP ( 'NONE', ( #9907, #5309, #17574, #7653 ) ) ;
#3761 = ADVANCED_FACE ( 'NONE', ( #7296 ), #12788, .F. ) ;
#3762 = ORIENTED_EDGE ( 'NONE', *, *, #21240, .T. ) ;
#3763 = ORIENTED_EDGE ( 'NONE', *, *, #18395, .F. ) ;
#3764 = FACE_OUTER_BOUND ( 'NONE', #13632, .T. ) ;
#3765 = ORIENTED_EDGE ( 'NONE', *, *, #3940, .T. ) ;
#3766 = ORIENTED_EDGE ( 'NONE', *, *, #20288, .T. ) ;
#3767 = EDGE_CURVE ( 'NONE', #13692, #11651, #10925, .T. ) ;
#3768 = FACE_OUTER_BOUND ( 'NONE', #3181, .T. ) ;
#3769 = AXIS2_PLACEMENT_3D ( 'NONE', #11283, #1445, #13258 ) ;
#3770 = VECTOR ( 'NONE', #13636, 1000.000000000000000 ) ;
#3771 = ORIENTED_EDGE ( 'NONE', *, *, #1108, .F. ) ;
#3772 = VECTOR ( 'NONE', #11024, 1000.000000000000000 ) ;
#3773 = DIRECTION ( 'NONE',  ( 0.000000000000000000, -0.3420201433256569445, -0.9396926207859126468 ) ) ;
#3774 = EDGE_CURVE ( 'NONE', #6248, #16691, #4500, .T. ) ;
#3775 = DIRECTION ( 'NONE',  ( -1.000000000000000000, -0.000000000000000000, 0.000000000000000000 ) ) ;
#3776 = DIRECTION ( 'NONE',  ( 0.000000000000000000, 0.000000000000000000, -1.000000000000000000 ) ) ;
#3777 = CARTESIAN_POINT ( 'NONE',  ( 5.000000000000002665, 18.94217447942673971, -85.93715160505934136 ) ) ;
#3778 = CARTESIAN_POINT ( 'NONE',  ( 10.00000000000000000, -3.728035544476815399, 84.97818067823770605 ) ) ;
#3779 = DIRECTION ( 'NONE',  ( 0.000000000000000000, 0.000000000000000000, -1.000000000000000000 ) ) ;
#3780 = DIRECTION ( 'NONE',  ( 0.000000000000000000, 8.943463253924873884E-15, -1.000000000000000000 ) ) ;
#3781 = ORIENTED_EDGE ( 'NONE', *, *, #20367, .T. ) ;
#3782 = AXIS2_PLACEMENT_3D ( 'NONE', #17457, #19214, #869 ) ;
#3783 = EDGE_CURVE ( 'NONE', #19526, #15663, #2020, .T. ) ;
#3784 = EDGE_CURVE ( 'NONE', #14878, #10281, #20729, .T. ) ;
#3785 = AXIS2_PLACEMENT_3D ( 'NONE', #4272, #2725, #7919 ) ;
#3786 = ADVANCED_FACE ( 'NONE', ( #4292 ), #3970, .F. ) ;
#3787 = AXIS2_PLACEMENT_3D ( 'NONE', #14561, #19864, #12907 ) ;
#3788 = CARTESIAN_POINT ( 'NONE',  ( 10.00000000000000000, 7.409634587003093742, 27.19958299168160565 ) ) ;
#3789 = ADVANCED_FACE ( 'NONE', ( #15678 ), #7616, .F. ) ;
#3790 = DIRECTION ( 'NONE',  ( 0.000000000000000000, 0.000000000000000000, 1.000000000000000000 ) ) ;
#3791 = EDGE_LOOP ( 'NONE', ( #6911, #9614, #12618, #20334 ) ) ;
#3792 = CARTESIAN_POINT ( 'NONE',  ( 10.00000000000000000, -36.60317927562525853, -76.78148674856802813 ) ) ;
#3793 = EDGE_LOOP ( 'NONE', ( #6220, #9218, #19397, #10336 ) ) ;
#3794 = CARTESIAN_POINT ( 'NONE',  ( 0.000000000000000000, 0.000000000000000000, 0.000000000000000000 ) ) ;
#3795 = VERTEX_POINT ( 'NONE', #7404 ) ;
#3796 = ORIENTED_EDGE ( 'NONE', *, *, #4354, .T. ) ;
#3797 = DIRECTION ( 'NONE',  ( 0.000000000000000000, 0.000000000000000000, -1.000000000000000000 ) ) ;
#3798 = LINE ( 'NONE', #7018, #16310 ) ;
#3799 = ADVANCED_FACE ( 'NONE', ( #14023 ), #20770, .F. ) ;
#3800 = CIRCLE ( 'NONE', #16146, 27.49900000000000233 ) ;
#3801 = CARTESIAN_POINT ( 'NONE',  ( 5.000000000000002665, -85.54350296776095774, -20.64725405482940346 ) ) ;
#3802 = CYLINDRICAL_SURFACE ( 'NONE', #5187, 45.00000000000000000 ) ;
#3803 = AXIS2_PLACEMENT_3D ( 'NONE', #10874, #14185, #20930 ) ;
#3804 = DIRECTION ( 'NONE',  ( 1.000000000000000000, 0.000000000000000000, 0.000000000000000000 ) ) ;
#3805 = CIRCLE ( 'NONE', #16147, 88.00000000000000000 ) ;
#3806 = LINE ( 'NONE', #3370, #5099 ) ;
#3807 = AXIS2_PLACEMENT_3D ( 'NONE', #9414, #17514, #1040 ) ;
#3808 = DIRECTION ( 'NONE',  ( -1.000000000000000000, 0.000000000000000000, 0.000000000000000000 ) ) ;
#3809 = EDGE_CURVE ( 'NONE', #15239, #8355, #4849, .T. ) ;
#3810 = DIRECTION ( 'NONE',  ( 0.000000000000000000, -1.000000000000000000, 0.000000000000000000 ) ) ;
#3811 = VERTEX_POINT ( 'NONE', #16332 ) ;
#3812 = AXIS2_PLACEMENT_3D ( 'NONE', #5224, #11962, #13829 ) ;
#3813 = DIRECTION ( 'NONE',  ( -1.000000000000000000, -0.000000000000000000, -0.000000000000000000 ) ) ;
#3814 = ORIENTED_EDGE ( 'NONE', *, *, #14224, .F. ) ;
#3815 = DIRECTION ( 'NONE',  ( 0.000000000000000000, -0.7431448254773861395, -0.6691306063588671194 ) ) ;
#3816 = EDGE_LOOP ( 'NONE', ( #15457, #471, #2459, #20302 ) ) ;
#3817 = CIRCLE ( 'NONE', #5589, 88.00000000000000000 ) ;
#3818 = EDGE_CURVE ( 'NONE', #8125, #21757, #11198, .T. ) ;
#3819 = CARTESIAN_POINT ( 'NONE',  ( 5.000000000000000000, -64.95266917914358373, 59.37298010462950515 ) ) ;
#3820 = AXIS2_PLACEMENT_3D ( 'NONE', #8008, #9754, #9968 ) ;
#3821 = AXIS2_PLACEMENT_3D ( 'NONE', #8279, #6745, #1973 ) ;
#3822 = DIRECTION ( 'NONE',  ( 1.000000000000000000, 0.000000000000000000, 0.000000000000000000 ) ) ;
#3823 = AXIS2_PLACEMENT_3D ( 'NONE', #11940, #15238, #113 ) ;
#3824 = ORIENTED_EDGE ( 'NONE', *, *, #21343, .T. ) ;
#3825 = ORIENTED_EDGE ( 'NONE', *, *, #9183, .F. ) ;
#3826 = ORIENTED_EDGE ( 'NONE', *, *, #4604, .T. ) ;
#3827 = VERTEX_POINT ( 'NONE', #1199 ) ;
#3828 = CARTESIAN_POINT ( 'NONE',  ( 10.00000000000000000, 0.000000000000000000, 0.000000000000000000 ) ) ;
#3829 = VERTEX_POINT ( 'NONE', #13122 ) ;
#3830 = EDGE_CURVE ( 'NONE', #286, #7680, #20021, .T. ) ;
#3831 = DIRECTION ( 'NONE',  ( 1.000000000000000000, 0.000000000000000000, 0.000000000000000000 ) ) ;
#3832 = CARTESIAN_POINT ( 'NONE',  ( 10.00000000000000000, -51.10509369859380513, -77.10190917907254970 ) ) ;
#3833 = CARTESIAN_POINT ( 'NONE',  ( 10.00000000000000000, 67.05625154133453236, 63.71729851637834940 ) ) ;
#3834 = EDGE_CURVE ( 'NONE', #7150, #14716, #10139, .T. ) ;
#3835 = CARTESIAN_POINT ( 'NONE',  ( -10.00000000000000000, 0.000000000000000000, 0.000000000000000000 ) ) ;
#3836 = DIRECTION ( 'NONE',  ( 0.000000000000000000, 0.000000000000000000, -1.000000000000000000 ) ) ;
#3837 = CIRCLE ( 'NONE', #11249, 6.500000000000000000 ) ;
#3838 = AXIS2_PLACEMENT_3D ( 'NONE', #12611, #19360, #7976 ) ;
#3839 = CYLINDRICAL_SURFACE ( 'NONE', #6126, 11.99999999999999822 ) ;
#3840 = EDGE_CURVE ( 'NONE', #12932, #173, #614, .T. ) ;
#3841 = AXIS2_PLACEMENT_3D ( 'NONE', #7067, #18448, #11702 ) ;
#3842 = ORIENTED_EDGE ( 'NONE', *, *, #1649, .F. ) ;
#3843 = AXIS2_PLACEMENT_3D ( 'NONE', #7506, #16001, #4195 ) ;
#3844 = EDGE_CURVE ( 'NONE', #17747, #14422, #7942, .T. ) ;
#3845 = DIRECTION ( 'NONE',  ( 1.000000000000000000, 0.000000000000000000, 0.000000000000000000 ) ) ;
#3846 = DIRECTION ( 'NONE',  ( -1.000000000000000000, -0.000000000000000000, -0.000000000000000000 ) ) ;
#3847 = LINE ( 'NONE', #7158, #8716 ) ;
#3848 = ORIENTED_EDGE ( 'NONE', *, *, #7755, .F. ) ;
#3849 = LINE ( 'NONE', #7387, #2782 ) ;
#3850 = ORIENTED_EDGE ( 'NONE', *, *, #567, .T. ) ;
#3851 = CARTESIAN_POINT ( 'NONE',  ( 0.000000000000000000, -68.93609746931198856, 54.69748134696436637 ) ) ;
#3852 = EDGE_LOOP ( 'NONE', ( #3468, #5746 ) ) ;
#3853 = ORIENTED_EDGE ( 'NONE', *, *, #5147, .F. ) ;
#3854 = CIRCLE ( 'NONE', #5975, 44.99999999999999289 ) ;
#3855 = AXIS2_PLACEMENT_3D ( 'NONE', #17877, #6284, #6057 ) ;
#3856 = DIRECTION ( 'NONE',  ( 0.000000000000000000, 0.000000000000000000, 1.000000000000000000 ) ) ;
#3857 = EDGE_LOOP ( 'NONE', ( #5946, #14474 ) ) ;
#3858 = CYLINDRICAL_SURFACE ( 'NONE', #17247, 44.99999999999999289 ) ;
#3859 = DIRECTION ( 'NONE',  ( 0.000000000000000000, 0.000000000000000000, -1.000000000000000000 ) ) ;
#3860 = DIRECTION ( 'NONE',  ( 0.000000000000000000, -0.9271838545667832054, -0.3746065934159226729 ) ) ;
#3861 = CARTESIAN_POINT ( 'NONE',  ( 0.000000000000000000, -26.27606311335958011, 10.21217444509402661 ) ) ;
#3862 = PRODUCT_DEFINITION_CONTEXT ( 'detailed design', #13334, 'design' ) ;
#3863 = DIRECTION ( 'NONE',  ( -1.000000000000000000, 0.000000000000000000, 0.000000000000000000 ) ) ;
#3864 = CARTESIAN_POINT ( 'NONE',  ( 10.00000000000000000, 0.000000000000000000, 0.000000000000000000 ) ) ;
#3865 = CARTESIAN_POINT ( 'NONE',  ( 10.00000000000000000, -31.75612719289743779, 3.943144139962448058 ) ) ;
#3866 = CIRCLE ( 'NONE', #2428, 1.100000000000017630 ) ;
#3867 = DIRECTION ( 'NONE',  ( 0.000000000000000000, 0.000000000000000000, -1.000000000000000000 ) ) ;
#3868 = DIRECTION ( 'NONE',  ( -1.000000000000000000, -0.000000000000000000, -0.000000000000000000 ) ) ;
#3869 = AXIS2_PLACEMENT_3D ( 'NONE', #13165, #15051, #9856 ) ;
#3870 = MECHANICAL_DESIGN_GEOMETRIC_PRESENTATION_REPRESENTATION (  '', ( #17280 ), #5626 ) ;
#3871 = ORIENTED_EDGE ( 'NONE', *, *, #3253, .F. ) ;
#3872 = AXIS2_PLACEMENT_3D ( 'NONE', #19837, #18197, #9662 ) ;
#3873 = CARTESIAN_POINT ( 'NONE',  ( 0.000000000000000000, 91.70173545986517638, 12.13370160540072007 ) ) ;
#3874 = VERTEX_POINT ( 'NONE', #13023 ) ;
#3875 = ORIENTED_EDGE ( 'NONE', *, *, #17699, .F. ) ;
#3876 = VERTEX_POINT ( 'NONE', #4731 ) ;
#3877 = LINE ( 'NONE', #10609, #10611 ) ;
#3878 = ORIENTED_EDGE ( 'NONE', *, *, #16757, .T. ) ;
#3879 = ORIENTED_EDGE ( 'NONE', *, *, #4229, .F. ) ;
#3880 = CARTESIAN_POINT ( 'NONE',  ( 10.00000000000000000, 0.000000000000000000, 0.000000000000000000 ) ) ;
#3881 = VERTEX_POINT ( 'NONE', #6185 ) ;
#3882 = CIRCLE ( 'NONE', #6730, 92.50100000000000477 ) ;
#3883 = DIRECTION ( 'NONE',  ( 1.000000000000000000, 0.000000000000000000, 0.000000000000000000 ) ) ;
#3884 = CYLINDRICAL_SURFACE ( 'NONE', #7496, 27.49900000000000233 ) ;
#3885 = CARTESIAN_POINT ( 'NONE',  ( 1.114299999999999846, 0.000000000000000000, 0.000000000000000000 ) ) ;
#3886 = DIRECTION ( 'NONE',  ( 0.000000000000000000, 0.000000000000000000, 1.000000000000000000 ) ) ;
#3887 = EDGE_CURVE ( 'NONE', #18262, #20717, #7328, .T. ) ;
#3888 = LINE ( 'NONE', #10727, #3417 ) ;
#3889 = DIRECTION ( 'NONE',  ( 0.000000000000000000, 0.000000000000000000, 1.000000000000000000 ) ) ;
#3890 = DIRECTION ( 'NONE',  ( 1.000000000000000000, 0.000000000000000000, 0.000000000000000000 ) ) ;
#3891 = CARTESIAN_POINT ( 'NONE',  ( 10.00000000000000000, 84.33453774737657227, 11.08490790852157559 ) ) ;
#3892 = ORIENTED_EDGE ( 'NONE', *, *, #21618, .F. ) ;
#3893 = EDGE_CURVE ( 'NONE', #14902, #13159, #4148, .T. ) ;
#3894 = CIRCLE ( 'NONE', #12, 3.000000000000000000 ) ;
#3895 = DIRECTION ( 'NONE',  ( 0.000000000000000000, 0.000000000000000000, 1.000000000000000000 ) ) ;
#3896 = CARTESIAN_POINT ( 'NONE',  ( 0.000000000000000000, 0.000000000000000000, 0.000000000000000000 ) ) ;
#3897 = ORIENTED_EDGE ( 'NONE', *, *, #20464, .F. ) ;
#3898 = CARTESIAN_POINT ( 'NONE',  ( 10.00000000000000000, 84.90234713953985590, 5.175025661884123274 ) ) ;
#3899 = ORIENTED_EDGE ( 'NONE', *, *, #8911, .T. ) ;
#3900 = SURFACE_STYLE_USAGE ( .BOTH. , #17284 ) ;
#3901 = DIRECTION ( 'NONE',  ( -1.000000000000000000, 0.000000000000000000, 0.000000000000000000 ) ) ;
#3902 = ORIENTED_EDGE ( 'NONE', *, *, #3947, .F. ) ;
#3903 = ORIENTED_EDGE ( 'NONE', *, *, #16774, .F. ) ;
#3904 = CARTESIAN_POINT ( 'NONE',  ( 0.000000000000000000, 0.000000000000000000, 0.000000000000000000 ) ) ;
#3905 = CARTESIAN_POINT ( 'NONE',  ( 10.00000000000000000, -82.02147376274702140, 42.76579056660835221 ) ) ;
#3906 = DIRECTION ( 'NONE',  ( 0.000000000000000000, 0.000000000000000000, 1.000000000000000000 ) ) ;
#3907 = DIRECTION ( 'NONE',  ( -1.000000000000000000, 0.000000000000000000, -0.000000000000000000 ) ) ;
#3908 = EDGE_CURVE ( 'NONE', #3086, #11509, #16503, .T. ) ;
#3909 = ADVANCED_FACE ( 'NONE', ( #9806 ), #16563, .F. ) ;
#3910 = DIRECTION ( 'NONE',  ( 0.000000000000000000, 0.000000000000000000, 1.000000000000000000 ) ) ;
#3911 = EDGE_CURVE ( 'NONE', #16436, #1002, #10484, .T. ) ;
#3912 = CIRCLE ( 'NONE', #730, 44.99999999999998579 ) ;
#3913 = DIRECTION ( 'NONE',  ( -1.000000000000000000, -0.000000000000000000, -0.000000000000000000 ) ) ;
#3914 = DIRECTION ( 'NONE',  ( 0.000000000000000000, 0.000000000000000000, 1.000000000000000000 ) ) ;
#3915 = CARTESIAN_POINT ( 'NONE',  ( 0.000000000000000000, 0.000000000000000000, 3.000000000000000000 ) ) ;
#3916 = EDGE_CURVE ( 'NONE', #6987, #20717, #7829, .T. ) ;
#3917 = ORIENTED_EDGE ( 'NONE', *, *, #11441, .T. ) ;
#3918 = CARTESIAN_POINT ( 'NONE',  ( 10.00000000000000000, 48.19312842678472464, 70.09002648625214249 ) ) ;
#3919 = ORIENTED_EDGE ( 'NONE', *, *, #7740, .T. ) ;
#3920 = EDGE_CURVE ( 'NONE', #14961, #4926, #3441, .T. ) ;
#3921 = CARTESIAN_POINT ( 'NONE',  ( 0.000000000000000000, 0.000000000000000000, 0.000000000000000000 ) ) ;
#3922 = ADVANCED_FACE ( 'NONE', ( #4036 ), #9435, .T. ) ;
#3923 = ORIENTED_EDGE ( 'NONE', *, *, #19982, .F. ) ;
#3924 = CARTESIAN_POINT ( 'NONE',  ( -8.900000000000019895, 1.469576158976824302E-14, 120.0000000000000284 ) ) ;
#3925 =( GEOMETRIC_REPRESENTATION_CONTEXT ( 3 ) GLOBAL_UNCERTAINTY_ASSIGNED_CONTEXT ( ( #11439 ) ) GLOBAL_UNIT_ASSIGNED_CONTEXT ( ( #13771, #12002, #13329 ) ) REPRESENTATION_CONTEXT ( 'NONE', 'WORKASPACE' ) );
#3926 = DIRECTION ( 'NONE',  ( -1.000000000000000000, -0.000000000000000000, -0.000000000000000000 ) ) ;
#3927 = ORIENTED_EDGE ( 'NONE', *, *, #12529, .F. ) ;
#3928 = EDGE_CURVE ( 'NONE', #16790, #17309, #18279, .T. ) ;
#3929 = ORIENTED_EDGE ( 'NONE', *, *, #9598, .T. ) ;
#3930 = ORIENTED_EDGE ( 'NONE', *, *, #8929, .F. ) ;
#3931 = ORIENTED_EDGE ( 'NONE', *, *, #10549, .T. ) ;
#3932 = CARTESIAN_POINT ( 'NONE',  ( 10.00000000000000000, 70.37753541436022431, -60.02863908169562279 ) ) ;
#3933 = ORIENTED_EDGE ( 'NONE', *, *, #957, .F. ) ;
#3934 = DIRECTION ( 'NONE',  ( 1.000000000000000000, 0.000000000000000000, 0.000000000000000000 ) ) ;
#3935 = FACE_BOUND ( 'NONE', #13386, .T. ) ;
#3936 = DIRECTION ( 'NONE',  ( 0.000000000000000000, 0.9993908270190957621, -0.03489949670249752750 ) ) ;
#3937 = EDGE_CURVE ( 'NONE', #14715, #2438, #1329, .T. ) ;
#3938 = FACE_OUTER_BOUND ( 'NONE', #3816, .T. ) ;
#3939 = CARTESIAN_POINT ( 'NONE',  ( -10.00000000000002309, 0.000000000000000000, 0.000000000000000000 ) ) ;
#3940 = EDGE_CURVE ( 'NONE', #21516, #19466, #829, .T. ) ;
#3941 = CYLINDRICAL_SURFACE ( 'NONE', #5393, 44.99999999999999289 ) ;
#3942 = AXIS2_PLACEMENT_3D ( 'NONE', #792, #9732, #17933 ) ;
#3943 = EDGE_LOOP ( 'NONE', ( #2513, #71, #17681, #8299 ) ) ;
#3944 = CARTESIAN_POINT ( 'NONE',  ( 0.000000000000000000, 51.18896083639267403, 71.57995730992199412 ) ) ;
#3945 = DIRECTION ( 'NONE',  ( -1.000000000000000000, -0.000000000000000000, -0.000000000000000000 ) ) ;
#3946 = DIRECTION ( 'NONE',  ( -1.000000000000000000, -0.000000000000000000, -0.000000000000000000 ) ) ;
#3947 = EDGE_CURVE ( 'NONE', #17904, #17373, #269, .T. ) ;
#3948 = ORIENTED_EDGE ( 'NONE', *, *, #10439, .T. ) ;
#3949 = CARTESIAN_POINT ( 'NONE',  ( 0.000000000000000000, 73.32282170386848463, 48.65967342042804944 ) ) ;
#3950 = ORIENTED_EDGE ( 'NONE', *, *, #18037, .F. ) ;
#3951 = CARTESIAN_POINT ( 'NONE',  ( 0.000000000000000000, -19.85071254963791176, 20.01672328094525000 ) ) ;
#3952 = EDGE_CURVE ( 'NONE', #21211, #16727, #620, .T. ) ;
#3953 = ORIENTED_EDGE ( 'NONE', *, *, #13959, .F. ) ;
#3954 = ORIENTED_EDGE ( 'NONE', *, *, #4350, .F. ) ;
#3955 = ORIENTED_EDGE ( 'NONE', *, *, #8246, .F. ) ;
#3956 = EDGE_CURVE ( 'NONE', #6083, #771, #941, .T. ) ;
#3957 = FACE_OUTER_BOUND ( 'NONE', #2771, .T. ) ;
#3958 = EDGE_CURVE ( 'NONE', #7513, #2166, #6984, .T. ) ;
#3959 = ORIENTED_EDGE ( 'NONE', *, *, #10613, .F. ) ;
#3960 = DIRECTION ( 'NONE',  ( 1.000000000000000000, 0.000000000000000000, 0.000000000000000000 ) ) ;
#3961 = CARTESIAN_POINT ( 'NONE',  ( 5.000000000000002665, -0.6609040254617754018, 87.99751818016873983 ) ) ;
#3962 = FACE_OUTER_BOUND ( 'NONE', #11662, .T. ) ;
#3963 = DIRECTION ( 'NONE',  ( 0.000000000000000000, 0.000000000000000000, 1.000000000000000000 ) ) ;
#3964 = AXIS2_PLACEMENT_3D ( 'NONE', #10312, #18942, #18506 ) ;
#3965 = LINE ( 'NONE', #10699, #11739 ) ;
#3966 = EDGE_CURVE ( 'NONE', #10355, #21543, #630, .T. ) ;
#3967 = DIRECTION ( 'NONE',  ( 1.000000000000000000, 0.000000000000000000, 0.000000000000000000 ) ) ;
#3968 = CARTESIAN_POINT ( 'NONE',  ( 5.000000000000000000, 61.60362715319035942, 62.84101464466265696 ) ) ;
#3969 = CIRCLE ( 'NONE', #17395, 44.99999999999999289 ) ;
#3970 = CYLINDRICAL_SURFACE ( 'NONE', #21071, 88.00000000000000000 ) ;
#3971 = CARTESIAN_POINT ( 'NONE',  ( 1.129531546211678616, 0.000000000000000000, -6.887500000000022382 ) ) ;
#3972 = ORIENTED_EDGE ( 'NONE', *, *, #17562, .F. ) ;
#3973 = CARTESIAN_POINT ( 'NONE',  ( 10.00000000000000000, 0.000000000000000000, 0.000000000000000000 ) ) ;
#3974 = ORIENTED_EDGE ( 'NONE', *, *, #8383, .F. ) ;
#3975 = AXIS2_PLACEMENT_3D ( 'NONE', #4210, #16137, #6204 ) ;
#3976 = VERTEX_POINT ( 'NONE', #17857 ) ;
#3977 = ORIENTED_EDGE ( 'NONE', *, *, #14096, .T. ) ;
#3978 = CARTESIAN_POINT ( 'NONE',  ( 0.000000000000000000, -74.39348546125087580, 54.97312363261390544 ) ) ;
#3979 = EDGE_LOOP ( 'NONE', ( #16898, #19968, #21454, #19203 ) ) ;
#3980 = ORIENTED_EDGE ( 'NONE', *, *, #13439, .F. ) ;
#3981 = CIRCLE ( 'NONE', #5756, 92.50100000000000477 ) ;
#3982 = EDGE_CURVE ( 'NONE', #10882, #8096, #11210, .T. ) ;
#3983 = DIRECTION ( 'NONE',  ( 1.000000000000000000, 0.000000000000000000, 0.000000000000000000 ) ) ;
#3984 = CIRCLE ( 'NONE', #5050, 92.50100000000000477 ) ;
#3985 = ORIENTED_EDGE ( 'NONE', *, *, #2455, .T. ) ;
#3986 = LINE ( 'NONE', #12595, #11818 ) ;
#3987 = FACE_OUTER_BOUND ( 'NONE', #10743, .T. ) ;
#3988 = CIRCLE ( 'NONE', #17766, 11.99999999999999822 ) ;
#3989 = DIRECTION ( 'NONE',  ( -1.000000000000000000, 0.000000000000000000, 0.000000000000000000 ) ) ;
#3990 = CARTESIAN_POINT ( 'NONE',  ( 0.000000000000000000, 0.000000000000000000, 0.000000000000000000 ) ) ;
#3991 = DIRECTION ( 'NONE',  ( 1.000000000000000000, 0.000000000000000000, 0.000000000000000000 ) ) ;
#3992 = CARTESIAN_POINT ( 'NONE',  ( 10.00000000000000000, -46.93287725819731548, -70.94007663282492615 ) ) ;
#3993 = CARTESIAN_POINT ( 'NONE',  ( 10.00000000000000000, 0.000000000000000000, 0.000000000000000000 ) ) ;
#3994 = DIRECTION ( 'NONE',  ( 0.000000000000000000, 0.000000000000000000, 1.000000000000000000 ) ) ;
#3995 = ORIENTED_EDGE ( 'NONE', *, *, #20133, .F. ) ;
#3996 = VECTOR ( 'NONE', #15935, 1000.000000000000000 ) ;
#3997 = LINE ( 'NONE', #14261, #19976 ) ;
#3998 = CIRCLE ( 'NONE', #12820, 44.99999999999998579 ) ;
#3999 = PLANE ( 'NONE',  #7015 ) ;
#4000 = CYLINDRICAL_SURFACE ( 'NONE', #19075, 120.0000000000000426 ) ;
#4001 = CIRCLE ( 'NONE', #6846, 88.00000000000000000 ) ;
#4002 = EDGE_LOOP ( 'NONE', ( #12148, #789, #19935, #6591 ) ) ;
#4003 = EDGE_CURVE ( 'NONE', #19412, #13513, #3800, .T. ) ;
#4004 = DIRECTION ( 'NONE',  ( 1.000000000000000000, 0.000000000000000000, 0.000000000000000000 ) ) ;
#4005 = ORIENTED_EDGE ( 'NONE', *, *, #2162, .F. ) ;
#4006 = VECTOR ( 'NONE', #15851, 1000.000000000000000 ) ;
#4007 = CARTESIAN_POINT ( 'NONE',  ( 0.000000000000000000, 87.58454185039441597, 8.540961822681984117 ) ) ;
#4008 = ORIENTED_EDGE ( 'NONE', *, *, #8300, .T. ) ;
#4009 = VERTEX_POINT ( 'NONE', #5924 ) ;
#4010 = DIRECTION ( 'NONE',  ( -1.000000000000000000, -0.000000000000000000, -0.000000000000000000 ) ) ;
#4011 = PRODUCT_DEFINITION ( 'UNKNOWN', '', #14538, #2101 ) ;
#4012 = AXIS2_PLACEMENT_3D ( 'NONE', #6113, #12833, #2465 ) ;
#4013 = CARTESIAN_POINT ( 'NONE',  ( 0.000000000000000000, 0.000000000000000000, 0.000000000000000000 ) ) ;
#4014 = DIRECTION ( 'NONE',  ( -1.000000000000000000, 0.000000000000000000, -0.000000000000000000 ) ) ;
#4015 = CARTESIAN_POINT ( 'NONE',  ( 10.00000000000000000, 0.000000000000000000, 0.000000000000000000 ) ) ;
#4016 = CARTESIAN_POINT ( 'NONE',  ( 0.000000000000000000, 0.000000000000000000, 0.000000000000000000 ) ) ;
#4017 = DIRECTION ( 'NONE',  ( -0.000000000000000000, -1.000000000000000000, -0.000000000000000000 ) ) ;
#4018 = LINE ( 'NONE', #171, #9212 ) ;
#4019 = EDGE_LOOP ( 'NONE', ( #9121, #15605, #9238, #18507 ) ) ;
#4020 = CARTESIAN_POINT ( 'NONE',  ( 0.000000000000000000, -81.97107881582211064, 22.71412948308539370 ) ) ;
#4021 = AXIS2_PLACEMENT_3D ( 'NONE', #2496, #14426, #12430 ) ;
#4022 = VERTEX_POINT ( 'NONE', #9327 ) ;
#4023 = CARTESIAN_POINT ( 'NONE',  ( 0.000000000000000000, 51.10509369859433804, 77.10190917907216601 ) ) ;
#4024 = ORIENTED_EDGE ( 'NONE', *, *, #17683, .T. ) ;
#4025 = FACE_OUTER_BOUND ( 'NONE', #13212, .T. ) ;
#4026 = EDGE_CURVE ( 'NONE', #6084, #18142, #732, .T. ) ;
#4027 = DIRECTION ( 'NONE',  ( 1.000000000000000000, 0.000000000000000000, 0.000000000000000000 ) ) ;
#4028 = ORIENTED_EDGE ( 'NONE', *, *, #15407, .T. ) ;
#4029 = SURFACE_STYLE_FILL_AREA ( #12326 ) ;
#4030 = CIRCLE ( 'NONE', #16388, 92.50100000000000477 ) ;
#4031 = ORIENTED_EDGE ( 'NONE', *, *, #2207, .T. ) ;
#4032 = ORIENTED_EDGE ( 'NONE', *, *, #1933, .F. ) ;
#4033 = AXIS2_PLACEMENT_3D ( 'NONE', #2122, #15590, #14145 ) ;
#4034 = ORIENTED_EDGE ( 'NONE', *, *, #5288, .T. ) ;
#4035 = DIRECTION ( 'NONE',  ( 0.000000000000000000, 0.000000000000000000, 1.000000000000000000 ) ) ;
#4036 = FACE_OUTER_BOUND ( 'NONE', #13707, .T. ) ;
#4037 = ADVANCED_FACE ( 'NONE', ( #16077 ), #19617, .T. ) ;
#4038 = VERTEX_POINT ( 'NONE', #14197 ) ;
#4039 = VECTOR ( 'NONE', #16846, 1000.000000000000000 ) ;
#4040 = CARTESIAN_POINT ( 'NONE',  ( 0.000000000000000000, 82.02147376274670876, 42.76579056660889933 ) ) ;
#4041 = CARTESIAN_POINT ( 'NONE',  ( 5.000000000000000000, -75.87763420127801339, -44.57111876559802255 ) ) ;
#4042 = CARTESIAN_POINT ( 'NONE',  ( 0.000000000000000000, 0.000000000000000000, 3.000000000000000000 ) ) ;
#4043 = CARTESIAN_POINT ( 'NONE',  ( 0.000000000000000000, -72.58367602204218372, 49.75550195834843237 ) ) ;
#4044 = VECTOR ( 'NONE', #13393, 1000.000000000000000 ) ;
#4045 = DIRECTION ( 'NONE',  ( -1.000000000000000000, 0.000000000000000000, 0.000000000000000000 ) ) ;
#4046 = EDGE_CURVE ( 'NONE', #12634, #15915, #7574, .T. ) ;
#4047 = VERTEX_POINT ( 'NONE', #20944 ) ;
#4048 = DIRECTION ( 'NONE',  ( 1.000000000000000000, -0.000000000000000000, 0.000000000000000000 ) ) ;
#4049 = CIRCLE ( 'NONE', #20978, 92.50099999999999056 ) ;
#4050 = CYLINDRICAL_SURFACE ( 'NONE', #6907, 12.00000000000000000 ) ;
#4051 = AXIS2_PLACEMENT_3D ( 'NONE', #18764, #13999, #8907 ) ;
#4052 = VECTOR ( 'NONE', #11459, 1000.000000000000000 ) ;
#4053 = DIRECTION ( 'NONE',  ( 0.000000000000000000, 0.000000000000000000, 1.000000000000000000 ) ) ;
#4054 = CIRCLE ( 'NONE', #14289, 11.99999999999999822 ) ;
#4055 = ORIENTED_EDGE ( 'NONE', *, *, #14466, .T. ) ;
#4056 = EDGE_CURVE ( 'NONE', #6639, #9318, #17219, .T. ) ;
#4057 = CARTESIAN_POINT ( 'NONE',  ( 0.000000000000000000, 0.000000000000000000, 0.000000000000000000 ) ) ;
#4058 = EDGE_CURVE ( 'NONE', #11265, #3283, #11217, .T. ) ;
#4059 = EDGE_CURVE ( 'NONE', #7682, #12369, #1058, .T. ) ;
#4060 = EDGE_LOOP ( 'NONE', ( #8800, #13133, #16514, #2587 ) ) ;
#4061 = DIRECTION ( 'NONE',  ( 1.000000000000000000, -0.000000000000000000, -0.000000000000000000 ) ) ;
#4062 = AXIS2_PLACEMENT_3D ( 'NONE', #11691, #13336, #6178 ) ;
#4063 = ORIENTED_EDGE ( 'NONE', *, *, #8257, .F. ) ;
#4064 = EDGE_CURVE ( 'NONE', #20840, #7792, #10154, .T. ) ;
#4065 = ORIENTED_EDGE ( 'NONE', *, *, #11624, .F. ) ;
#4066 = VERTEX_POINT ( 'NONE', #18477 ) ;
#4067 = CARTESIAN_POINT ( 'NONE',  ( 10.00000000000000000, -45.60224695560514618, -80.47900393021774335 ) ) ;
#4068 = VERTEX_POINT ( 'NONE', #13487 ) ;
#4069 = CARTESIAN_POINT ( 'NONE',  ( 0.000000000000000000, 61.60362715319035942, 62.84101464466265696 ) ) ;
#4070 = DIRECTION ( 'NONE',  ( -0.8831157194574072999, 5.745494457773168027E-17, -0.4691552259617553511 ) ) ;
#4071 = DIRECTION ( 'NONE',  ( 0.000000000000000000, 0.000000000000000000, 1.000000000000000000 ) ) ;
#4072 = CIRCLE ( 'NONE', #15711, 88.00000000000000000 ) ;
#4073 = AXIS2_PLACEMENT_3D ( 'NONE', #7700, #11121, #15883 ) ;
#4074 = AXIS2_PLACEMENT_3D ( 'NONE', #5668, #903, #21138 ) ;
#4075 = CYLINDRICAL_SURFACE ( 'NONE', #815, 92.50100000000000477 ) ;
#4076 = AXIS2_PLACEMENT_3D ( 'NONE', #12012, #7145, #1847 ) ;
#4077 = EDGE_CURVE ( 'NONE', #7508, #13187, #6563, .T. ) ;
#4078 = TOROIDAL_SURFACE ( 'NONE', #17142, 5.100000000000000533, 0.09999999999999971412 ) ;
#4079 = CYLINDRICAL_SURFACE ( 'NONE', #14923, 44.99999999999998579 ) ;
#4080 = DIRECTION ( 'NONE',  ( 0.000000000000000000, -0.4067366430757887730, -0.9135454576426059736 ) ) ;
#4081 = CYLINDRICAL_SURFACE ( 'NONE', #18873, 44.99999999999998579 ) ;
#4082 = DIRECTION ( 'NONE',  ( 0.000000000000000000, 0.000000000000000000, 1.000000000000000000 ) ) ;
#4083 = EDGE_CURVE ( 'NONE', #21518, #1477, #12973, .T. ) ;
#4084 = DIRECTION ( 'NONE',  ( 0.000000000000000000, 0.000000000000000000, 1.000000000000000000 ) ) ;
#4085 = AXIS2_PLACEMENT_3D ( 'NONE', #3150, #2824, #19826 ) ;
#4086 = EDGE_CURVE ( 'NONE', #21782, #5377, #11584, .T. ) ;
#4087 = AXIS2_PLACEMENT_3D ( 'NONE', #15709, #6997, #2015 ) ;
#4088 = DIRECTION ( 'NONE',  ( -1.000000000000000000, -0.000000000000000000, -0.000000000000000000 ) ) ;
#4089 = ORIENTED_EDGE ( 'NONE', *, *, #13808, .T. ) ;
#4090 = CIRCLE ( 'NONE', #3032, 100.0000000000000000 ) ;
#4091 = VERTEX_POINT ( 'NONE', #1793 ) ;
#4092 = VECTOR ( 'NONE', #19603, 1000.000000000000000 ) ;
#4093 = AXIS2_PLACEMENT_3D ( 'NONE', #6806, #20390, #7022 ) ;
#4094 = VERTEX_POINT ( 'NONE', #3008 ) ;
#4095 = CIRCLE ( 'NONE', #12906, 27.49900000000000233 ) ;
#4096 = EDGE_CURVE ( 'NONE', #9115, #18608, #15088, .T. ) ;
#4097 = ORIENTED_EDGE ( 'NONE', *, *, #11338, .F. ) ;
#4098 = ORIENTED_EDGE ( 'NONE', *, *, #3313, .F. ) ;
#4099 = LINE ( 'NONE', #1104, #3122 ) ;
#4100 = ORIENTED_EDGE ( 'NONE', *, *, #1521, .F. ) ;
#4101 = CARTESIAN_POINT ( 'NONE',  ( 10.00000000000000000, 24.17932380791747349, -20.96092317126980831 ) ) ;
#4102 = CYLINDRICAL_SURFACE ( 'NONE', #14188, 92.50100000000000477 ) ;
#4103 = CARTESIAN_POINT ( 'NONE',  ( 10.00000000000000000, 81.83745710415318797, -32.35167097270070258 ) ) ;
#4104 = CYLINDRICAL_SURFACE ( 'NONE', #20925, 44.99999999999998579 ) ;
#4105 = AXIS2_PLACEMENT_3D ( 'NONE', #5643, #12370, #17353 ) ;
#4106 = DIRECTION ( 'NONE',  ( 0.000000000000000000, 0.8290375725550428454, -0.5591929034707450175 ) ) ;
#4107 = ADVANCED_FACE ( 'NONE', ( #129 ), #20028, .T. ) ;
#4108 = AXIS2_PLACEMENT_3D ( 'NONE', #13830, #13727, #12171 ) ;
#4109 = CYLINDRICAL_SURFACE ( 'NONE', #17852, 44.99999999999999289 ) ;
#4110 = CYLINDRICAL_SURFACE ( 'NONE', #6264, 92.50100000000000477 ) ;
#4111 = DIRECTION ( 'NONE',  ( 1.000000000000000000, 0.000000000000000000, 0.000000000000000000 ) ) ;
#4112 = ADVANCED_FACE ( 'NONE', ( #18591 ), #9850, .F. ) ;
#4113 = ORIENTED_EDGE ( 'NONE', *, *, #15420, .T. ) ;
#4114 = ADVANCED_FACE ( 'NONE', ( #21675 ), #3221, .F. ) ;
#4115 = DIRECTION ( 'NONE',  ( 1.000000000000000000, 0.000000000000000000, 0.000000000000000000 ) ) ;
#4116 = CARTESIAN_POINT ( 'NONE',  ( 10.00000000000000000, 84.79630770241077187, 6.691460262316813790 ) ) ;
#4117 = CARTESIAN_POINT ( 'NONE',  ( 10.00000000000000000, -74.39348546125016526, -54.97312363261490731 ) ) ;
#4118 = CIRCLE ( 'NONE', #19290, 32.00000000000000000 ) ;
#4119 = EDGE_LOOP ( 'NONE', ( #13160, #10114, #16005, #20641 ) ) ;
#4120 = CIRCLE ( 'NONE', #16468, 88.00000000000000000 ) ;
#4121 = DIRECTION ( 'NONE',  ( -1.000000000000000000, 0.000000000000000000, 0.000000000000000000 ) ) ;
#4122 = ORIENTED_EDGE ( 'NONE', *, *, #12560, .T. ) ;
#4123 = COLOUR_RGB ( '', 0.72549020, 0.75294118, 0.79215686) ;
#4124 = CARTESIAN_POINT ( 'NONE',  ( 0.000000000000000000, 60.00000000000000000, -15.00000000000000000 ) ) ;
#4125 = ORIENTED_EDGE ( 'NONE', *, *, #12182, .F. ) ;
#4126 = ORIENTED_EDGE ( 'NONE', *, *, #17274, .F. ) ;
#4127 = CARTESIAN_POINT ( 'NONE',  ( 0.000000000000000000, 0.000000000000000000, 0.000000000000000000 ) ) ;
#4128 = DIRECTION ( 'NONE',  ( 0.000000000000000000, 0.7431448254773953543, -0.6691306063588567943 ) ) ;
#4129 = CARTESIAN_POINT ( 'NONE',  ( 0.000000000000000000, 0.000000000000000000, 0.000000000000000000 ) ) ;
#4130 = CARTESIAN_POINT ( 'NONE',  ( 5.000000000000000000, 13.56333590714055681, -28.98337314858420299 ) ) ;
#4131 = CARTESIAN_POINT ( 'NONE',  ( 0.000000000000000000, 46.89573839703386682, -79.73220629831438089 ) ) ;
#4132 = CARTESIAN_POINT ( 'NONE',  ( 10.00000000000000000, 21.31452625070926743, 82.34610137166127686 ) ) ;
#4133 = CARTESIAN_POINT ( 'NONE',  ( -10.00000000000000000, 0.000000000000000000, 0.000000000000000000 ) ) ;
#4134 = CARTESIAN_POINT ( 'NONE',  ( 0.000000000000000000, 41.89587599971545018, 77.38692120905484728 ) ) ;
#4135 = CARTESIAN_POINT ( 'NONE',  ( 10.00000000000000000, 27.26034713664097353, -7.182859710736244629 ) ) ;
#4136 = AXIS2_PLACEMENT_3D ( 'NONE', #13044, #21769, #8186 ) ;
#4137 = CIRCLE ( 'NONE', #962, 27.49900000000000233 ) ;
#4138 = ORIENTED_EDGE ( 'NONE', *, *, #584, .F. ) ;
#4139 = AXIS2_PLACEMENT_3D ( 'NONE', #8836, #17778, #4080 ) ;
#4140 = CARTESIAN_POINT ( 'NONE',  ( 0.000000000000000000, 3.728035544476225649, 84.97818067823770605 ) ) ;
#4141 = ORIENTED_EDGE ( 'NONE', *, *, #20775, .F. ) ;
#4142 = DIRECTION ( 'NONE',  ( -1.000000000000000000, -0.000000000000000000, -0.000000000000000000 ) ) ;
#4143 = ORIENTED_EDGE ( 'NONE', *, *, #9428, .T. ) ;
#4144 = CARTESIAN_POINT ( 'NONE',  ( 0.000000000000000000, -4.294029059349679045, -27.86182539015970505 ) ) ;
#4145 = DIRECTION ( 'NONE',  ( 0.000000000000000000, -0.1391731009600725710, 0.9902680687415692518 ) ) ;
#4146 = ORIENTED_EDGE ( 'NONE', *, *, #19774, .F. ) ;
#4147 =( NAMED_UNIT ( * ) SI_UNIT ( $, .STERADIAN. ) SOLID_ANGLE_UNIT ( ) );
#4148 = CIRCLE ( 'NONE', #6282, 44.99999999999999289 ) ;
#4149 = ORIENTED_EDGE ( 'NONE', *, *, #7188, .T. ) ;
#4150 = VERTEX_POINT ( 'NONE', #8526 ) ;
#4151 = TOROIDAL_SURFACE ( 'NONE', #20040, 101.1000000000000369, 1.100000000000002087 ) ;
#4152 = ORIENTED_EDGE ( 'NONE', *, *, #17106, .F. ) ;
#4153 = DIRECTION ( 'NONE',  ( -1.000000000000000000, 0.000000000000000000, 0.000000000000000000 ) ) ;
#4154 = CARTESIAN_POINT ( 'NONE',  ( 10.00000000000000000, 81.97107881582226696, -22.71412948308482171 ) ) ;
#4155 = ORIENTED_EDGE ( 'NONE', *, *, #9092, .F. ) ;
#4156 = LINE ( 'NONE', #13988, #16373 ) ;
#4157 = DIRECTION ( 'NONE',  ( 0.000000000000000000, 0.000000000000000000, 1.000000000000000000 ) ) ;
#4158 = DIRECTION ( 'NONE',  ( 0.000000000000000000, 0.000000000000000000, 1.000000000000000000 ) ) ;
#4159 = LINE ( 'NONE', #14204, #19179 ) ;
#4160 = DIRECTION ( 'NONE',  ( -1.000000000000000000, 0.000000000000000000, 0.000000000000000000 ) ) ;
#4161 = EDGE_CURVE ( 'NONE', #6607, #7559, #19912, .T. ) ;
#4162 = ORIENTED_EDGE ( 'NONE', *, *, #7045, .T. ) ;
#4163 = CARTESIAN_POINT ( 'NONE',  ( 0.000000000000000000, 0.000000000000000000, 15.00000000000000000 ) ) ;
#4164 = CIRCLE ( 'NONE', #977, 44.99999999999998579 ) ;
#4165 = CARTESIAN_POINT ( 'NONE',  ( 10.00000000000000000, 25.17124263951009411, -12.69364185792227495 ) ) ;
#4166 = AXIS2_PLACEMENT_3D ( 'NONE', #6789, #16950, #7005 ) ;
#4167 = AXIS2_PLACEMENT_3D ( 'NONE', #18975, #15317, #8807 ) ;
#4168 = CIRCLE ( 'NONE', #982, 92.50100000000000477 ) ;
#4169 = EDGE_CURVE ( 'NONE', #4447, #6087, #4164, .T. ) ;
#4170 = CARTESIAN_POINT ( 'NONE',  ( 10.00000000000000000, 0.000000000000000000, 0.000000000000000000 ) ) ;
#4171 = ORIENTED_EDGE ( 'NONE', *, *, #13221, .T. ) ;
#4172 = DIRECTION ( 'NONE',  ( -1.000000000000000000, -0.000000000000000000, -0.000000000000000000 ) ) ;
#4173 = ORIENTED_EDGE ( 'NONE', *, *, #1262, .F. ) ;
#4174 = DIRECTION ( 'NONE',  ( 0.000000000000000000, 0.000000000000000000, -1.000000000000000000 ) ) ;
#4175 = ORIENTED_EDGE ( 'NONE', *, *, #8531, .F. ) ;
#4176 = ORIENTED_EDGE ( 'NONE', *, *, #9350, .T. ) ;
#4177 = ORIENTED_EDGE ( 'NONE', *, *, #16896, .F. ) ;
#4178 = DIRECTION ( 'NONE',  ( 0.000000000000000000, 0.9271838545667883125, -0.3746065934159096833 ) ) ;
#4179 = ORIENTED_EDGE ( 'NONE', *, *, #6665, .T. ) ;
#4180 = CARTESIAN_POINT ( 'NONE',  ( -1.500000000000001332, 0.000000000000000000, -6.728125000000022560 ) ) ;
#4181 = CIRCLE ( 'NONE', #16534, 88.00000000000000000 ) ;
#4182 = DIRECTION ( 'NONE',  ( 0.000000000000000000, -0.5877852522924797984, 0.8090169943749424553 ) ) ;
#4183 = DIRECTION ( 'NONE',  ( -1.000000000000000000, 0.000000000000000000, 0.000000000000000000 ) ) ;
#4184 = VECTOR ( 'NONE', #4061, 1000.000000000000000 ) ;
#4185 = CIRCLE ( 'NONE', #18318, 11.99999999999999645 ) ;
#4186 = CIRCLE ( 'NONE', #7019, 44.99999999999998579 ) ;
#4187 = DIRECTION ( 'NONE',  ( 0.000000000000000000, 0.000000000000000000, 1.000000000000000000 ) ) ;
#4188 = CARTESIAN_POINT ( 'NONE',  ( 0.000000000000000000, 0.000000000000000000, 0.000000000000000000 ) ) ;
#4189 = EDGE_CURVE ( 'NONE', #5507, #839, #15254, .T. ) ;
#4190 = CARTESIAN_POINT ( 'NONE',  ( -1.129531546211723025, 6.886005254585696675E-16, 5.612499999999999822 ) ) ;
#4191 = ADVANCED_FACE ( 'NONE', ( #6880 ), #1354, .T. ) ;
#4192 = DIRECTION ( 'NONE',  ( 1.000000000000000000, 0.000000000000000000, 0.000000000000000000 ) ) ;
#4193 = EDGE_CURVE ( 'NONE', #9671, #17337, #10499, .T. ) ;
#4194 = DIRECTION ( 'NONE',  ( 1.000000000000000000, 0.000000000000000000, 0.000000000000000000 ) ) ;
#4195 = DIRECTION ( 'NONE',  ( 0.000000000000000000, 1.063963731932441790E-14, -1.000000000000000000 ) ) ;
#4196 = ADVANCED_FACE ( 'NONE', ( #13161 ), #6674, .F. ) ;
#4197 = CYLINDRICAL_SURFACE ( 'NONE', #15048, 92.50100000000000477 ) ;
#4198 = ORIENTED_EDGE ( 'NONE', *, *, #19627, .T. ) ;
#4199 = AXIS2_PLACEMENT_3D ( 'NONE', #4946, #21614, #21520 ) ;
#4200 = VERTEX_POINT ( 'NONE', #11729 ) ;
#4201 = AXIS2_PLACEMENT_3D ( 'NONE', #8912, #19194, #15770 ) ;
#4202 = ORIENTED_EDGE ( 'NONE', *, *, #1218, .T. ) ;
#4203 = EDGE_CURVE ( 'NONE', #6246, #20166, #8399, .T. ) ;
#4204 = ORIENTED_EDGE ( 'NONE', *, *, #18162, .F. ) ;
#4205 = ORIENTED_EDGE ( 'NONE', *, *, #742, .T. ) ;
#4206 = EDGE_CURVE ( 'NONE', #771, #21218, #5229, .T. ) ;
#4207 = DIRECTION ( 'NONE',  ( 0.000000000000000000, 0.000000000000000000, 1.000000000000000000 ) ) ;
#4208 = EDGE_LOOP ( 'NONE', ( #19197, #7078, #18584, #1612 ) ) ;
#4209 = DIRECTION ( 'NONE',  ( -1.000000000000000000, 0.000000000000000000, -0.000000000000000000 ) ) ;
#4210 = CARTESIAN_POINT ( 'NONE',  ( -1.399999999999998579, 0.000000000000000000, 0.000000000000000000 ) ) ;
#4211 = CIRCLE ( 'NONE', #11970, 92.50100000000000477 ) ;
#4212 = DIRECTION ( 'NONE',  ( -1.000000000000000000, 0.000000000000000000, 0.000000000000000000 ) ) ;
#4213 = DIRECTION ( 'NONE',  ( 1.000000000000000000, 0.000000000000000000, 0.000000000000000000 ) ) ;
#4214 = AXIS2_PLACEMENT_3D ( 'NONE', #14523, #10880, #19609 ) ;
#4215 = CARTESIAN_POINT ( 'NONE',  ( 0.000000000000000000, 84.19736439813806328, 38.30455363800960811 ) ) ;
#4216 = VECTOR ( 'NONE', #20851, 1000.000000000000000 ) ;
#4217 = CYLINDRICAL_SURFACE ( 'NONE', #14326, 27.49900000000000233 ) ;
#4218 = DIRECTION ( 'NONE',  ( 1.000000000000000000, 0.000000000000000000, 0.000000000000000000 ) ) ;
#4219 = DIRECTION ( 'NONE',  ( 0.000000000000000000, 0.000000000000000000, 1.000000000000000000 ) ) ;
#4220 = ADVANCED_FACE ( 'NONE', ( #6775 ), #18914, .T. ) ;
#4221 = ORIENTED_EDGE ( 'NONE', *, *, #3523, .F. ) ;
#4222 = CARTESIAN_POINT ( 'NONE',  ( 10.00000000000000000, -83.48638250753209888, -27.82128566055197538 ) ) ;
#4223 = CARTESIAN_POINT ( 'NONE',  ( 10.00000000000000000, 0.000000000000000000, 0.000000000000000000 ) ) ;
#4224 = EDGE_CURVE ( 'NONE', #3550, #21750, #9060, .T. ) ;
#4225 = CARTESIAN_POINT ( 'NONE',  ( 0.000000000000000000, 21.31452625071037943, -82.34610137166097843 ) ) ;
#4226 = ORIENTED_EDGE ( 'NONE', *, *, #18289, .F. ) ;
#4227 = DIRECTION ( 'NONE',  ( -1.000000000000000000, 0.000000000000000000, 0.000000000000000000 ) ) ;
#4228 = ORIENTED_EDGE ( 'NONE', *, *, #12409, .F. ) ;
#4229 = EDGE_CURVE ( 'NONE', #10281, #7770, #21091, .T. ) ;
#4230 = AXIS2_PLACEMENT_3D ( 'NONE', #14436, #1067, #19741 ) ;
#4231 = ORIENTED_EDGE ( 'NONE', *, *, #6542, .F. ) ;
#4232 = CARTESIAN_POINT ( 'NONE',  ( 0.000000000000000000, 0.000000000000000000, 0.000000000000000000 ) ) ;
#4233 = DIRECTION ( 'NONE',  ( 0.000000000000000000, 0.8660254037844397068, -0.4999999999999980016 ) ) ;
#4234 = ORIENTED_EDGE ( 'NONE', *, *, #19701, .T. ) ;
#4235 = ORIENTED_EDGE ( 'NONE', *, *, #9411, .F. ) ;
#4236 = EDGE_CURVE ( 'NONE', #21231, #935, #11928, .T. ) ;
#4237 = DIRECTION ( 'NONE',  ( -1.000000000000000000, 0.000000000000000000, 0.000000000000000000 ) ) ;
#4238 = FACE_OUTER_BOUND ( 'NONE', #4721, .T. ) ;
#4239 = ADVANCED_FACE ( 'NONE', ( #3768 ), #10392, .F. ) ;
#4240 = CYLINDRICAL_SURFACE ( 'NONE', #10047, 88.00000000000000000 ) ;
#4241 = CARTESIAN_POINT ( 'NONE',  ( 10.00000000000000000, 0.000000000000000000, 0.000000000000000000 ) ) ;
#4242 = FACE_OUTER_BOUND ( 'NONE', #9294, .T. ) ;
#4243 = CARTESIAN_POINT ( 'NONE',  ( -10.00000000000000000, 0.000000000000000000, 0.000000000000000000 ) ) ;
#4244 = CARTESIAN_POINT ( 'NONE',  ( 6.123233995736766282E-16, 100.0000000000000000, 5.000000000000000000 ) ) ;
#4245 = FACE_OUTER_BOUND ( 'NONE', #16699, .T. ) ;
#4246 = DIRECTION ( 'NONE',  ( 0.000000000000000000, 0.000000000000000000, -1.000000000000000000 ) ) ;
#4247 = EDGE_CURVE ( 'NONE', #17357, #12772, #8754, .T. ) ;
#4248 = AXIS2_PLACEMENT_3D ( 'NONE', #12823, #9511, #4554 ) ;
#4249 = ORIENTED_EDGE ( 'NONE', *, *, #16050, .T. ) ;
#4250 = CARTESIAN_POINT ( 'NONE',  ( 10.00000000000000000, 0.000000000000000000, 0.000000000000000000 ) ) ;
#4251 = ORIENTED_EDGE ( 'NONE', *, *, #7043, .F. ) ;
#4252 = DIRECTION ( 'NONE',  ( -1.000000000000000000, 0.000000000000000000, 0.000000000000000000 ) ) ;
#4253 = ORIENTED_EDGE ( 'NONE', *, *, #9866, .F. ) ;
#4254 = DIRECTION ( 'NONE',  ( 1.000000000000000000, 0.000000000000000000, 0.000000000000000000 ) ) ;
#4255 = CYLINDRICAL_SURFACE ( 'NONE', #2107, 92.50100000000000477 ) ;
#4256 = VERTEX_POINT ( 'NONE', #20566 ) ;
#4257 = ORIENTED_EDGE ( 'NONE', *, *, #18133, .T. ) ;
#4258 = ORIENTED_EDGE ( 'NONE', *, *, #3245, .T. ) ;
#4259 = VERTEX_POINT ( 'NONE', #19023 ) ;
#4260 = AXIS2_PLACEMENT_3D ( 'NONE', #16811, #6555, #10179 ) ;
#4261 = FACE_BOUND ( 'NONE', #11573, .T. ) ;
#4262 = DIRECTION ( 'NONE',  ( 1.000000000000000000, -0.000000000000000000, -0.000000000000000000 ) ) ;
#4263 = ORIENTED_EDGE ( 'NONE', *, *, #5454, .F. ) ;
#4264 = CARTESIAN_POINT ( 'NONE',  ( 10.00000000000000000, 0.000000000000000000, 0.000000000000000000 ) ) ;
#4265 = CARTESIAN_POINT ( 'NONE',  ( 6.123233995736766282E-16, 0.000000000000000000, 5.000000000000000000 ) ) ;
#4266 = DIRECTION ( 'NONE',  ( 0.000000000000000000, 0.000000000000000000, 1.000000000000000000 ) ) ;
#4267 = CARTESIAN_POINT ( 'NONE',  ( 0.000000000000000000, -12.46320060045744071, 29.47318494484024853 ) ) ;
#4268 = LINE ( 'NONE', #12548, #5970 ) ;
#4269 = VERTEX_POINT ( 'NONE', #13719 ) ;
#4270 = DIRECTION ( 'NONE',  ( -1.000000000000000000, 0.000000000000000000, 0.000000000000000000 ) ) ;
#4271 = CARTESIAN_POINT ( 'NONE',  ( 5.000000000000000000, -57.06999622551850138, 66.98518889142063415 ) ) ;
#4272 = CARTESIAN_POINT ( 'NONE',  ( 0.000000000000000000, 0.000000000000000000, 0.000000000000000000 ) ) ;
#4273 = ORIENTED_EDGE ( 'NONE', *, *, #2825, .T. ) ;
#4274 = CARTESIAN_POINT ( 'NONE',  ( 0.000000000000000000, -39.87723064937174655, 83.46401306393555330 ) ) ;
#4275 = VERTEX_POINT ( 'NONE', #10505 ) ;
#4276 = DIRECTION ( 'NONE',  ( 0.000000000000000000, 0.3420201433256693235, -0.9396926207859080948 ) ) ;
#4277 = ORIENTED_EDGE ( 'NONE', *, *, #9581, .T. ) ;
#4278 = ORIENTED_EDGE ( 'NONE', *, *, #14484, .F. ) ;
#4279 = EDGE_CURVE ( 'NONE', #2625, #3525, #20404, .T. ) ;
#4280 = ORIENTED_EDGE ( 'NONE', *, *, #7355, .F. ) ;
#4281 = CARTESIAN_POINT ( 'NONE',  ( 1.500000000000000000, 0.000000000000000000, 15.00000000000000000 ) ) ;
#4282 = ORIENTED_EDGE ( 'NONE', *, *, #15080, .T. ) ;
#4283 = CYLINDRICAL_SURFACE ( 'NONE', #13723, 11.99999999999999822 ) ;
#4284 = CARTESIAN_POINT ( 'NONE',  ( 10.00000000000000000, 84.19736439813806328, 38.30455363800960811 ) ) ;
#4285 = DIRECTION ( 'NONE',  ( -1.000000000000000000, -0.000000000000000000, -0.000000000000000000 ) ) ;
#4286 = COLOUR_RGB ( '', 0.08235294, 0.09019608, 0.10196078) ;
#4287 = CARTESIAN_POINT ( 'NONE',  ( 10.00000000000000000, -26.69209308833503513, -6.612652082459592684 ) ) ;
#4288 = EDGE_CURVE ( 'NONE', #9061, #5771, #8054, .T. ) ;
#4289 = DIRECTION ( 'NONE',  ( -1.000000000000000000, -0.000000000000000000, -0.000000000000000000 ) ) ;
#4290 = CARTESIAN_POINT ( 'NONE',  ( 10.00000000000000000, 29.29369617358468858, 87.74003855418408193 ) ) ;
#4291 = DIRECTION ( 'NONE',  ( -1.000000000000000000, -0.000000000000000000, -0.000000000000000000 ) ) ;
#4292 = FACE_OUTER_BOUND ( 'NONE', #8195, .T. ) ;
#4293 = CYLINDRICAL_SURFACE ( 'NONE', #14792, 44.99999999999998579 ) ;
#4294 = DIRECTION ( 'NONE',  ( 0.000000000000000000, 0.000000000000000000, 1.000000000000000000 ) ) ;
#4295 = ORIENTED_EDGE ( 'NONE', *, *, #8354, .T. ) ;
#4296 = ORIENTED_EDGE ( 'NONE', *, *, #5671, .F. ) ;
#4297 = EDGE_LOOP ( 'NONE', ( #2592, #3, #10888, #20448 ) ) ;
#4298 = ADVANCED_BREP_SHAPE_REPRESENTATION ( '', ( #20897, #15567 ), #4640 ) ;
#4299 = ORIENTED_EDGE ( 'NONE', *, *, #18242, .T. ) ;
#4300 = EDGE_CURVE ( 'NONE', #49, #5950, #5935, .T. ) ;
#4301 = ORIENTED_EDGE ( 'NONE', *, *, #14507, .F. ) ;
#4302 = CARTESIAN_POINT ( 'NONE',  ( -5.000000000000000000, 8.660254037844385522, 9.999999999999998224 ) ) ;
#4303 = VECTOR ( 'NONE', #10637, 1000.000000000000000 ) ;
#4304 = ORIENTED_EDGE ( 'NONE', *, *, #3656, .T. ) ;
#4305 = CARTESIAN_POINT ( 'NONE',  ( 1.500000000000000000, -7.000000000000000000, 15.00000000000000000 ) ) ;
#4306 = CARTESIAN_POINT ( 'NONE',  ( 0.000000000000000000, -77.39385041987173963, 35.28996114464576550 ) ) ;
#4307 = FACE_OUTER_BOUND ( 'NONE', #7904, .T. ) ;
#4308 = DIRECTION ( 'NONE',  ( 0.000000000000000000, 0.000000000000000000, 1.000000000000000000 ) ) ;
#4309 = DIRECTION ( 'NONE',  ( 1.000000000000000000, 0.000000000000000000, 0.000000000000000000 ) ) ;
#4310 = DIRECTION ( 'NONE',  ( 0.000000000000000000, 0.000000000000000000, -1.000000000000000000 ) ) ;
#4311 = CARTESIAN_POINT ( 'NONE',  ( 0.000000000000000000, 61.71252885873388294, 58.53847642588613809 ) ) ;
#4312 = DIRECTION ( 'NONE',  ( 0.000000000000000000, 0.000000000000000000, 1.000000000000000000 ) ) ;
#4313 = EDGE_CURVE ( 'NONE', #20799, #15070, #14380, .T. ) ;
#4314 = DIRECTION ( 'NONE',  ( -1.000000000000000000, -0.000000000000000000, -0.000000000000000000 ) ) ;
#4315 = AXIS2_PLACEMENT_3D ( 'NONE', #20246, #5109, #20143 ) ;
#4316 = VERTEX_POINT ( 'NONE', #7310 ) ;
#4317 = EDGE_CURVE ( 'NONE', #21664, #14408, #10288, .T. ) ;
#4318 = DIRECTION ( 'NONE',  ( 0.000000000000000000, 0.000000000000000000, 1.000000000000000000 ) ) ;
#4319 = ORIENTED_EDGE ( 'NONE', *, *, #18289, .T. ) ;
#4320 = CIRCLE ( 'NONE', #16314, 27.49900000000000588 ) ;
#4321 = FACE_OUTER_BOUND ( 'NONE', #3378, .T. ) ;
#4322 = CARTESIAN_POINT ( 'NONE',  ( 10.00000000000000000, 31.15801000616834315, 79.14775961996400611 ) ) ;
#4323 = EDGE_CURVE ( 'NONE', #14098, #7892, #19353, .T. ) ;
#4324 = ORIENTED_EDGE ( 'NONE', *, *, #21635, .F. ) ;
#4325 = EDGE_CURVE ( 'NONE', #6904, #12778, #9446, .T. ) ;
#4326 = EDGE_CURVE ( 'NONE', #2438, #6675, #2763, .T. ) ;
#4327 = LINE ( 'NONE', #17605, #4900 ) ;
#4328 = VERTEX_POINT ( 'NONE', #568 ) ;
#4329 = VERTEX_POINT ( 'NONE', #18707 ) ;
#4330 = DIRECTION ( 'NONE',  ( -1.244140434411257678E-18, -1.000000000000000000, -2.355105825922269596E-16 ) ) ;
#4331 = LINE ( 'NONE', #16374, #3636 ) ;
#4332 = EDGE_CURVE ( 'NONE', #2463, #16061, #7100, .T. ) ;
#4333 = VECTOR ( 'NONE', #1334, 1000.000000000000000 ) ;
#4334 = ORIENTED_EDGE ( 'NONE', *, *, #14960, .F. ) ;
#4335 = VERTEX_POINT ( 'NONE', #3557 ) ;
#4336 = DIRECTION ( 'NONE',  ( 1.000000000000000000, 0.000000000000000000, 0.000000000000000000 ) ) ;
#4337 = LINE ( 'NONE', #17940, #19039 ) ;
#4338 = AXIS2_PLACEMENT_3D ( 'NONE', #2875, #18130, #9270 ) ;
#4339 = VECTOR ( 'NONE', #10368, 1000.000000000000000 ) ;
#4340 = DIRECTION ( 'NONE',  ( 1.000000000000000000, 0.000000000000000000, 0.000000000000000000 ) ) ;
#4341 = DIRECTION ( 'NONE',  ( -1.000000000000000000, 0.000000000000000000, -0.000000000000000000 ) ) ;
#4342 = DIRECTION ( 'NONE',  ( 1.000000000000000000, 0.000000000000000000, 0.000000000000000000 ) ) ;
#4343 = CARTESIAN_POINT ( 'NONE',  ( 10.00000000000000000, 0.000000000000000000, 0.000000000000000000 ) ) ;
#4344 = FACE_OUTER_BOUND ( 'NONE', #16758, .T. ) ;
#4345 = CARTESIAN_POINT ( 'NONE',  ( 10.00000000000000000, -73.32282170386882569, 48.65967342042752364 ) ) ;
#4346 = EDGE_CURVE ( 'NONE', #17286, #16668, #12377, .T. ) ;
#4347 = DIRECTION ( 'NONE',  ( -1.000000000000000000, -0.000000000000000000, 0.000000000000000000 ) ) ;
#4348 = ORIENTED_EDGE ( 'NONE', *, *, #18814, .T. ) ;
#4349 = EDGE_CURVE ( 'NONE', #20466, #11655, #2075, .T. ) ;
#4350 = EDGE_CURVE ( 'NONE', #8942, #21012, #3470, .T. ) ;
#4351 = DIRECTION ( 'NONE',  ( 1.000000000000000000, 0.000000000000000000, 0.000000000000000000 ) ) ;
#4352 = AXIS2_PLACEMENT_3D ( 'NONE', #8488, #20097, #21853 ) ;
#4353 = ORIENTED_EDGE ( 'NONE', *, *, #14178, .F. ) ;
#4354 = EDGE_CURVE ( 'NONE', #21233, #11274, #4099, .T. ) ;
#4355 = CARTESIAN_POINT ( 'NONE',  ( 0.000000000000000000, 52.34334029047981574, -76.26670130689429072 ) ) ;
#4356 = VECTOR ( 'NONE', #14348, 1000.000000000000000 ) ;
#4357 = CYLINDRICAL_SURFACE ( 'NONE', #1758, 44.99999999999998579 ) ;
#4358 = CYLINDRICAL_SURFACE ( 'NONE', #17629, 27.49900000000000233 ) ;
#4359 = EDGE_LOOP ( 'NONE', ( #12673, #7785, #8044, #18086 ) ) ;
#4360 = AXIS2_PLACEMENT_3D ( 'NONE', #17090, #10338, #1952 ) ;
#4361 = SURFACE_SIDE_STYLE ('',( #6370 ) ) ;
#4362 = ORIENTED_EDGE ( 'NONE', *, *, #7850, .T. ) ;
#4363 = EDGE_CURVE ( 'NONE', #6056, #15522, #21808, .T. ) ;
#4364 = EDGE_LOOP ( 'NONE', ( #9900, #9756, #21495, #2533 ) ) ;
#4365 = ORIENTED_EDGE ( 'NONE', *, *, #7836, .T. ) ;
#4366 = CARTESIAN_POINT ( 'NONE',  ( 0.000000000000000000, -17.64925110578526812, 86.21197095186339254 ) ) ;
#4367 = CARTESIAN_POINT ( 'NONE',  ( 10.00000000000000000, 78.01214607583800387, -33.90124636420030413 ) ) ;
#4368 = ORIENTED_EDGE ( 'NONE', *, *, #8818, .F. ) ;
#4369 = EDGE_CURVE ( 'NONE', #11040, #13984, #12993, .T. ) ;
#4370 = VECTOR ( 'NONE', #18075, 1000.000000000000000 ) ;
#4371 = CARTESIAN_POINT ( 'NONE',  ( 10.00000000000000000, 71.33759994382042180, -58.88447872958914786 ) ) ;
#4372 = CARTESIAN_POINT ( 'NONE',  ( -1.500000000000001332, 0.000000000000000000, 0.000000000000000000 ) ) ;
#4373 = DIRECTION ( 'NONE',  ( 1.000000000000000000, -0.000000000000000000, 0.000000000000000000 ) ) ;
#4374 = CARTESIAN_POINT ( 'NONE',  ( 0.000000000000000000, 0.000000000000000000, 0.000000000000000000 ) ) ;
#4375 = CARTESIAN_POINT ( 'NONE',  ( 1.139999999999995239, 0.000000000000000000, 0.000000000000000000 ) ) ;
#4376 = CIRCLE ( 'NONE', #13897, 12.00000000000000178 ) ;
#4377 = ORIENTED_EDGE ( 'NONE', *, *, #20533, .F. ) ;
#4378 = ADVANCED_FACE ( 'NONE', ( #18022 ), #9589, .F. ) ;
#4379 = AXIS2_PLACEMENT_3D ( 'NONE', #7468, #19287, #14310 ) ;
#4380 = LINE ( 'NONE', #11330, #16582 ) ;
#4381 = LINE ( 'NONE', #19410, #1964 ) ;
#4382 = VERTEX_POINT ( 'NONE', #7630 ) ;
#4383 = ADVANCED_FACE ( 'NONE', ( #9165 ), #19233, .F. ) ;
#4384 = CARTESIAN_POINT ( 'NONE',  ( -1.500000000000000000, 5.000000000000000000, 7.000000000000000000 ) ) ;
#4385 = ORIENTED_EDGE ( 'NONE', *, *, #8949, .F. ) ;
#4386 = AXIS2_PLACEMENT_3D ( 'NONE', #9773, #8025, #11436 ) ;
#4387 = PLANE ( 'NONE',  #3855 ) ;
#4388 = DIRECTION ( 'NONE',  ( 1.000000000000000000, 0.000000000000000000, 0.000000000000000000 ) ) ;
#4389 = EDGE_LOOP ( 'NONE', ( #9965, #7681 ) ) ;
#4390 = DIRECTION ( 'NONE',  ( -1.000000000000000000, -0.000000000000000000, -0.000000000000000000 ) ) ;
#4391 = AXIS2_PLACEMENT_3D ( 'NONE', #13090, #7799, #14757 ) ;
#4392 = ORIENTED_EDGE ( 'NONE', *, *, #7869, .T. ) ;
#4393 = ORIENTED_EDGE ( 'NONE', *, *, #20113, .T. ) ;
#4394 = ORIENTED_EDGE ( 'NONE', *, *, #2825, .F. ) ;
#4395 = DIRECTION ( 'NONE',  ( -1.000000000000000000, 0.000000000000000000, 0.000000000000000000 ) ) ;
#4396 = VECTOR ( 'NONE', #1030, 1000.000000000000000 ) ;
#4397 = EDGE_LOOP ( 'NONE', ( #5760, #17278, #1072, #17639 ) ) ;
#4398 = DIRECTION ( 'NONE',  ( 0.000000000000000000, -0.7880107536067275653, 0.6156614753256510753 ) ) ;
#4399 = DIRECTION ( 'NONE',  ( 0.000000000000000000, 0.2756373558169997184, -0.9612616959383185611 ) ) ;
#4400 = DIRECTION ( 'NONE',  ( -1.000000000000000000, 0.000000000000000000, 0.000000000000000000 ) ) ;
#4401 =( NAMED_UNIT ( * ) SI_UNIT ( $, .STERADIAN. ) SOLID_ANGLE_UNIT ( ) );
#4402 = DIRECTION ( 'NONE',  ( 0.000000000000000000, 0.000000000000000000, 1.000000000000000000 ) ) ;
#4403 = CIRCLE ( 'NONE', #13926, 113.8250000000000171 ) ;
#4404 = DIRECTION ( 'NONE',  ( 0.000000000000000000, 0.7880107536067190166, 0.6156614753256620665 ) ) ;
#4405 = EDGE_CURVE ( 'NONE', #9323, #1046, #20884, .T. ) ;
#4406 = AXIS2_PLACEMENT_3D ( 'NONE', #20312, #19553, #11583 ) ;
#4407 = CARTESIAN_POINT ( 'NONE',  ( -90.00000000000000000, 0.000000000000000000, 0.000000000000000000 ) ) ;
#4408 = CARTESIAN_POINT ( 'NONE',  ( 1.499999999999999556, 7.400000000000020783, 0.000000000000000000 ) ) ;
#4409 = AXIS2_PLACEMENT_3D ( 'NONE', #11983, #15514, #6804 ) ;
#4410 = AXIS2_PLACEMENT_3D ( 'NONE', #12360, #647, #14228 ) ;
#4411 = DIRECTION ( 'NONE',  ( 0.000000000000000000, 0.000000000000000000, 1.000000000000000000 ) ) ;
#4412 = ORIENTED_EDGE ( 'NONE', *, *, #1218, .F. ) ;
#4413 = ORIENTED_EDGE ( 'NONE', *, *, #6950, .T. ) ;
#4414 = VERTEX_POINT ( 'NONE', #4302 ) ;
#4415 = ORIENTED_EDGE ( 'NONE', *, *, #6650, .F. ) ;
#4416 = AXIS2_PLACEMENT_3D ( 'NONE', #21155, #4461, #12741 ) ;
#4417 = CIRCLE ( 'NONE', #4786, 92.50100000000000477 ) ;
#4418 = AXIS2_PLACEMENT_3D ( 'NONE', #18934, #6901, #13841 ) ;
#4419 = AXIS2_PLACEMENT_3D ( 'NONE', #15876, #9124, #4266 ) ;
#4420 = ORIENTED_EDGE ( 'NONE', *, *, #16251, .T. ) ;
#4421 = CIRCLE ( 'NONE', #188, 11.99999999999999822 ) ;
#4422 = CARTESIAN_POINT ( 'NONE',  ( 10.00000000000000000, 17.70753755129037188, 21.03896658273978559 ) ) ;
#4423 = ORIENTED_EDGE ( 'NONE', *, *, #2528, .T. ) ;
#4424 = DIRECTION ( 'NONE',  ( -1.000000000000000000, 0.000000000000000000, 0.000000000000000000 ) ) ;
#4425 = CARTESIAN_POINT ( 'NONE',  ( 0.000000000000000000, -52.34334029047821701, -76.26670130689538496 ) ) ;
#4426 = CARTESIAN_POINT ( 'NONE',  ( 5.000000000000000000, 27.40684453873966575, 16.51862198942017557 ) ) ;
#4427 = CYLINDRICAL_SURFACE ( 'NONE', #13599, 11.99999999999999822 ) ;
#4428 = CYLINDRICAL_SURFACE ( 'NONE', #3127, 11.99999999999999822 ) ;
#4429 = FACE_OUTER_BOUND ( 'NONE', #8717, .T. ) ;
#4430 = CIRCLE ( 'NONE', #5843, 44.99999999999999289 ) ;
#4431 = CYLINDRICAL_SURFACE ( 'NONE', #14674, 88.00000000000000000 ) ;
#4432 = FACE_OUTER_BOUND ( 'NONE', #19077, .T. ) ;
#4433 = CARTESIAN_POINT ( 'NONE',  ( 0.000000000000000000, 19.83954325428771881, -82.71385593638672162 ) ) ;
#4434 = EDGE_CURVE ( 'NONE', #12524, #11232, #5955, .T. ) ;
#4435 = AXIS2_PLACEMENT_3D ( 'NONE', #13318, #4941, #11675 ) ;
#4436 = ORIENTED_EDGE ( 'NONE', *, *, #15759, .T. ) ;
#4437 = AXIS2_PLACEMENT_3D ( 'NONE', #2812, #2579, #9310 ) ;
#4438 = AXIS2_PLACEMENT_3D ( 'NONE', #18945, #3804, #5146 ) ;
#4439 = CYLINDRICAL_SURFACE ( 'NONE', #11143, 88.00000000000000000 ) ;
#4440 = ORIENTED_EDGE ( 'NONE', *, *, #19607, .T. ) ;
#4441 = EDGE_CURVE ( 'NONE', #15239, #2267, #10514, .T. ) ;
#4442 = CYLINDRICAL_SURFACE ( 'NONE', #10878, 44.99999999999999289 ) ;
#4443 = DIRECTION ( 'NONE',  ( 1.000000000000000000, 0.000000000000000000, -0.000000000000000000 ) ) ;
#4444 = ORIENTED_EDGE ( 'NONE', *, *, #1369, .F. ) ;
#4445 = DIRECTION ( 'NONE',  ( 0.000000000000000000, -0.2079116908177664480, 0.9781476007338041345 ) ) ;
#4446 = ORIENTED_EDGE ( 'NONE', *, *, #12270, .F. ) ;
#4447 = VERTEX_POINT ( 'NONE', #12481 ) ;
#4448 = APPLICATION_PROTOCOL_DEFINITION ( 'draft international standard', 'automotive_design', 1998, #2331 ) ;
#4449 = EDGE_CURVE ( 'NONE', #21353, #12424, #17941, .T. ) ;
#4450 = CARTESIAN_POINT ( 'NONE',  ( 10.00000000000000000, -45.60224695560626174, 80.47900393021710386 ) ) ;
#4451 = ORIENTED_EDGE ( 'NONE', *, *, #17967, .T. ) ;
#4452 = AXIS2_PLACEMENT_3D ( 'NONE', #3322, #5095, #21663 ) ;
#4453 = ORIENTED_EDGE ( 'NONE', *, *, #9757, .F. ) ;
#4454 = CARTESIAN_POINT ( 'NONE',  ( -90.00000000000000000, 1.393954219129474843E-14, 113.8250000000000028 ) ) ;
#4455 = CARTESIAN_POINT ( 'NONE',  ( 0.000000000000000000, 2.481790431839256517, 92.46770094066594936 ) ) ;
#4456 = CARTESIAN_POINT ( 'NONE',  ( 0.000000000000000000, 0.000000000000000000, 15.00000000000000000 ) ) ;
#4457 = CARTESIAN_POINT ( 'NONE',  ( 5.000000000000002665, -24.89070495400677530, -84.40647372620527733 ) ) ;
#4458 = DIRECTION ( 'NONE',  ( 0.000000000000000000, 0.000000000000000000, 1.000000000000000000 ) ) ;
#4459 = CARTESIAN_POINT ( 'NONE',  ( 10.00000000000000000, 82.02147376274669455, 42.76579056660889933 ) ) ;
#4460 = FACE_BOUND ( 'NONE', #3391, .T. ) ;
#4461 = DIRECTION ( 'NONE',  ( 1.000000000000000000, 0.000000000000000000, 0.000000000000000000 ) ) ;
#4462 = DIRECTION ( 'NONE',  ( -1.000000000000000000, 0.000000000000000000, 0.000000000000000000 ) ) ;
#4463 = ADVANCED_FACE ( 'NONE', ( #19549 ), #10936, .F. ) ;
#4464 = EDGE_CURVE ( 'NONE', #5258, #8125, #9264, .T. ) ;
#4465 = EDGE_CURVE ( 'NONE', #20877, #15560, #16882, .T. ) ;
#4466 = ORIENTED_EDGE ( 'NONE', *, *, #10419, .F. ) ;
#4467 = LINE ( 'NONE', #2693, #16440 ) ;
#4468 = EDGE_CURVE ( 'NONE', #13478, #21353, #3817, .T. ) ;
#4469 = EDGE_LOOP ( 'NONE', ( #19467, #8016, #2581, #20382 ) ) ;
#4470 = AXIS2_PLACEMENT_3D ( 'NONE', #6521, #3084, #11478 ) ;
#4471 = VECTOR ( 'NONE', #15705, 1000.000000000000000 ) ;
#4472 = DIRECTION ( 'NONE',  ( 0.000000000000000000, -0.8660254037844432595, 0.4999999999999918954 ) ) ;
#4473 = FILL_AREA_STYLE_COLOUR ( '', #2108 ) ;
#4474 = CARTESIAN_POINT ( 'NONE',  ( 0.000000000000000000, 0.000000000000000000, 0.000000000000000000 ) ) ;
#4475 = ORIENTED_EDGE ( 'NONE', *, *, #15927, .F. ) ;
#4476 =( NAMED_UNIT ( * ) PLANE_ANGLE_UNIT ( ) SI_UNIT ( $, .RADIAN. ) );
#4477 = ADVANCED_FACE ( 'NONE', ( #2770 ), #15914, .T. ) ;
#4478 = ORIENTED_EDGE ( 'NONE', *, *, #11468, .T. ) ;
#4479 = ORIENTED_EDGE ( 'NONE', *, *, #13496, .T. ) ;
#4480 = EDGE_LOOP ( 'NONE', ( #14543, #18450, #20484, #15425 ) ) ;
#4481 = DIRECTION ( 'NONE',  ( -1.000000000000000000, 0.000000000000000000, 0.000000000000000000 ) ) ;
#4482 = DIRECTION ( 'NONE',  ( -0.000000000000000000, -0.000000000000000000, -1.000000000000000000 ) ) ;
#4483 = ORIENTED_EDGE ( 'NONE', *, *, #2566, .T. ) ;
#4484 = EDGE_CURVE ( 'NONE', #14902, #20191, #5984, .T. ) ;
#4485 = CIRCLE ( 'NONE', #4136, 44.99999999999999289 ) ;
#4486 = PLANE ( 'NONE',  #1566 ) ;
#4487 = CARTESIAN_POINT ( 'NONE',  ( 10.00000000000000000, 0.000000000000000000, 0.000000000000000000 ) ) ;
#4488 = AXIS2_PLACEMENT_3D ( 'NONE', #9342, #5943, #10790 ) ;
#4489 = DIRECTION ( 'NONE',  ( 0.000000000000000000, 0.000000000000000000, 1.000000000000000000 ) ) ;
#4490 = CARTESIAN_POINT ( 'NONE',  ( 10.00000000000000000, 87.44637528609661103, 9.855528870798920593 ) ) ;
#4491 = AXIS2_PLACEMENT_3D ( 'NONE', #16914, #11, #10487 ) ;
#4492 = CARTESIAN_POINT ( 'NONE',  ( 10.00000000000000000, 0.000000000000000000, 0.000000000000000000 ) ) ;
#4493 = EDGE_LOOP ( 'NONE', ( #9287, #18058, #16909, #16289 ) ) ;
#4494 = DIRECTION ( 'NONE',  ( 0.000000000000000000, -0.5877852522924797984, 0.8090169943749425663 ) ) ;
#4495 = ADVANCED_FACE ( 'NONE', ( #881 ), #7841, .F. ) ;
#4496 = CARTESIAN_POINT ( 'NONE',  ( -1.140000000000000124, 6.898680348956876061E-16, 5.633200000000004870 ) ) ;
#4497 = VERTEX_POINT ( 'NONE', #12920 ) ;
#4498 = CYLINDRICAL_SURFACE ( 'NONE', #2021, 32.00000000000000000 ) ;
#4499 = ORIENTED_EDGE ( 'NONE', *, *, #14040, .F. ) ;
#4500 = CIRCLE ( 'NONE', #18621, 11.99999999999999822 ) ;
#4501 = DIRECTION ( 'NONE',  ( 0.000000000000000000, 0.000000000000000000, -1.000000000000000000 ) ) ;
#4502 = AXIS2_PLACEMENT_3D ( 'NONE', #609, #15953, #21262 ) ;
#4503 = DIRECTION ( 'NONE',  ( -1.000000000000000000, -0.000000000000000000, -0.000000000000000000 ) ) ;
#4504 = AXIS2_PLACEMENT_3D ( 'NONE', #17952, #12633, #9203 ) ;
#4505 = ORIENTED_EDGE ( 'NONE', *, *, #8779, .F. ) ;
#4506 = DIRECTION ( 'NONE',  ( 1.000000000000000000, 0.000000000000000000, 0.000000000000000000 ) ) ;
#4507 = CIRCLE ( 'NONE', #7332, 92.50100000000000477 ) ;
#4508 = EDGE_CURVE ( 'NONE', #4068, #20507, #1213, .T. ) ;
#4509 = ORIENTED_EDGE ( 'NONE', *, *, #4847, .F. ) ;
#4510 = ORIENTED_EDGE ( 'NONE', *, *, #2609, .T. ) ;
#4511 = CYLINDRICAL_SURFACE ( 'NONE', #17473, 44.99999999999998579 ) ;
#4512 = EDGE_CURVE ( 'NONE', #17030, #13577, #11596, .T. ) ;
#4513 = ORIENTED_EDGE ( 'NONE', *, *, #4894, .F. ) ;
#4514 = DIRECTION ( 'NONE',  ( -1.000000000000000000, -0.000000000000000000, 0.000000000000000000 ) ) ;
#4515 = LINE ( 'NONE', #14668, #16039 ) ;
#4516 = FACE_OUTER_BOUND ( 'NONE', #6701, .T. ) ;
#4517 = EDGE_CURVE ( 'NONE', #5352, #1972, #1706, .T. ) ;
#4518 = DIRECTION ( 'NONE',  ( 1.000000000000000000, 0.000000000000000000, 0.000000000000000000 ) ) ;
#4519 = ADVANCED_FACE ( 'NONE', ( #21547 ), #6530, .T. ) ;
#4520 = VECTOR ( 'NONE', #3117, 1000.000000000000000 ) ;
#4521 = DIRECTION ( 'NONE',  ( -1.000000000000000000, 0.000000000000000000, 0.000000000000000000 ) ) ;
#4522 = CARTESIAN_POINT ( 'NONE',  ( 10.00000000000000000, 84.12297548659721258, 32.40974838672968872 ) ) ;
#4523 = CIRCLE ( 'NONE', #21800, 105.0992000000000104 ) ;
#4524 = CIRCLE ( 'NONE', #16866, 44.99999999999999289 ) ;
#4525 = CARTESIAN_POINT ( 'NONE',  ( 0.000000000000000000, -52.96496548042899377, 66.55750800669339640 ) ) ;
#4526 = CARTESIAN_POINT ( 'NONE',  ( 5.000000000000000000, 19.29292659244040564, -25.53004080487742300 ) ) ;
#4527 = AXIS2_PLACEMENT_3D ( 'NONE', #3664, #10398, #17152 ) ;
#4528 = DIRECTION ( 'NONE',  ( 0.000000000000000000, 0.000000000000000000, -1.000000000000000000 ) ) ;
#4529 = ORIENTED_EDGE ( 'NONE', *, *, #11108, .T. ) ;
#4530 = ORIENTED_EDGE ( 'NONE', *, *, #20039, .F. ) ;
#4531 = ORIENTED_EDGE ( 'NONE', *, *, #9320, .T. ) ;
#4532 = VECTOR ( 'NONE', #3091, 1000.000000000000000 ) ;
#4533 = EDGE_LOOP ( 'NONE', ( #21623, #16487, #3115, #21701 ) ) ;
#4534 = CIRCLE ( 'NONE', #18659, 88.00000000000000000 ) ;
#4535 = VECTOR ( 'NONE', #6668, 1000.000000000000000 ) ;
#4536 = AXIS2_PLACEMENT_3D ( 'NONE', #12814, #21228, #7325 ) ;
#4537 = ORIENTED_EDGE ( 'NONE', *, *, #17011, .F. ) ;
#4538 = CARTESIAN_POINT ( 'NONE',  ( -10.00000000000000000, 0.000000000000000000, 0.000000000000000000 ) ) ;
#4539 = VERTEX_POINT ( 'NONE', #2976 ) ;
#4540 = LINE ( 'NONE', #7959, #9233 ) ;
#4541 = DIRECTION ( 'NONE',  ( 1.000000000000000000, 0.000000000000000000, 0.000000000000000000 ) ) ;
#4542 = DIRECTION ( 'NONE',  ( 1.000000000000000000, 0.000000000000000000, 0.000000000000000000 ) ) ;
#4543 = FACE_OUTER_BOUND ( 'NONE', #18434, .T. ) ;
#4544 = DIRECTION ( 'NONE',  ( 0.000000000000000000, 0.2079116908177597312, -0.9781476007338054668 ) ) ;
#4545 = CYLINDRICAL_SURFACE ( 'NONE', #13659, 44.99999999999999289 ) ;
#4546 = CARTESIAN_POINT ( 'NONE',  ( 0.000000000000000000, 41.89587599971653731, -77.38692120905427885 ) ) ;
#4547 = VECTOR ( 'NONE', #11018, 1000.000000000000000 ) ;
#4548 = VECTOR ( 'NONE', #14115, 1000.000000000000000 ) ;
#4549 = ORIENTED_EDGE ( 'NONE', *, *, #15717, .F. ) ;
#4550 = AXIS2_PLACEMENT_3D ( 'NONE', #19986, #21744, #9690 ) ;
#4551 = CARTESIAN_POINT ( 'NONE',  ( 2.000000000000000000, 67.00000000000000000, 9.999999999999998224 ) ) ;
#4552 = EDGE_LOOP ( 'NONE', ( #15827, #10119, #5327, #8191 ) ) ;
#4553 = FACE_BOUND ( 'NONE', #10873, .T. ) ;
#4554 = DIRECTION ( 'NONE',  ( 0.000000000000000000, 0.000000000000000000, 1.000000000000000000 ) ) ;
#4555 = EDGE_LOOP ( 'NONE', ( #10212, #7117, #8225, #4005 ) ) ;
#4556 = CARTESIAN_POINT ( 'NONE',  ( 10.00000000000000000, 81.32027326007924728, -44.08455690948972716 ) ) ;
#4557 = ORIENTED_EDGE ( 'NONE', *, *, #14901, .T. ) ;
#4558 = ORIENTED_EDGE ( 'NONE', *, *, #9027, .F. ) ;
#4559 = CARTESIAN_POINT ( 'NONE',  ( 0.000000000000000000, 0.000000000000000000, 0.000000000000000000 ) ) ;
#4560 = VECTOR ( 'NONE', #21468, 1000.000000000000000 ) ;
#4561 = CARTESIAN_POINT ( 'NONE',  ( 10.00000000000000000, 2.208823992044147033, 85.03123271466937183 ) ) ;
#4562 = ORIENTED_EDGE ( 'NONE', *, *, #1236, .F. ) ;
#4563 = EDGE_CURVE ( 'NONE', #8013, #12830, #1541, .T. ) ;
#4564 = CIRCLE ( 'NONE', #12674, 45.00000000000000711 ) ;
#4565 = ORIENTED_EDGE ( 'NONE', *, *, #18915, .F. ) ;
#4566 = CARTESIAN_POINT ( 'NONE',  ( 10.00000000000000000, 12.94633825542266869, 24.26081875733338933 ) ) ;
#4567 = AXIS2_PLACEMENT_3D ( 'NONE', #10785, #19299, #5828 ) ;
#4568 = LINE ( 'NONE', #21248, #14801 ) ;
#4569 = CARTESIAN_POINT ( 'NONE',  ( 10.00000000000000000, -56.35896156214997887, 73.34918167666290856 ) ) ;
#4570 = CARTESIAN_POINT ( 'NONE',  ( -1.200000000000006617, 0.000000000000000000, 0.000000000000000000 ) ) ;
#4571 = LINE ( 'NONE', #11303, #6234 ) ;
#4572 = CARTESIAN_POINT ( 'NONE',  ( -10.00000000000000000, 0.000000000000000000, 0.000000000000000000 ) ) ;
#4573 = EDGE_CURVE ( 'NONE', #215, #18043, #7358, .T. ) ;
#4574 = CARTESIAN_POINT ( 'NONE',  ( 10.00000000000000000, 0.000000000000000000, 0.000000000000000000 ) ) ;
#4575 = CARTESIAN_POINT ( 'NONE',  ( 5.000000000000000000, 41.89587599971545728, 77.38692120905484728 ) ) ;
#4576 = CARTESIAN_POINT ( 'NONE',  ( 10.00000000000000000, 0.000000000000000000, 0.000000000000000000 ) ) ;
#4577 = SHAPE_REPRESENTATION ( 'planetary rotating cover', ( #15567 ), #3229 ) ;
#4578 = ORIENTED_EDGE ( 'NONE', *, *, #5120, .F. ) ;
#4579 = CIRCLE ( 'NONE', #14102, 6.728125000000022560 ) ;
#4580 = VERTEX_POINT ( 'NONE', #6752 ) ;
#4581 = AXIS2_PLACEMENT_3D ( 'NONE', #12293, #5451, #8760 ) ;
#4582 = CARTESIAN_POINT ( 'NONE',  ( 5.000000000000000888, -6.063030049134863653, -31.42037024962131397 ) ) ;
#4583 =( NAMED_UNIT ( * ) PLANE_ANGLE_UNIT ( ) SI_UNIT ( $, .RADIAN. ) );
#4584 = CARTESIAN_POINT ( 'NONE',  ( 10.00000000000000000, -41.21966518006011881, 82.80926399530274296 ) ) ;
#4585 = EDGE_LOOP ( 'NONE', ( #11923, #10689, #21215, #18356 ) ) ;
#4586 = ORIENTED_EDGE ( 'NONE', *, *, #1933, .T. ) ;
#4587 = VERTEX_POINT ( 'NONE', #4859 ) ;
#4588 = EDGE_CURVE ( 'NONE', #17903, #536, #16675, .T. ) ;
#4589 = ADVANCED_FACE ( 'NONE', ( #19780 ), #16908, .F. ) ;
#4590 = VERTEX_POINT ( 'NONE', #6320 ) ;
#4591 = DIRECTION ( 'NONE',  ( -1.000000000000000000, 0.000000000000000000, -0.000000000000000000 ) ) ;
#4592 = CARTESIAN_POINT ( 'NONE',  ( 10.00000000000000000, 83.03980459022454852, 18.42770452393382641 ) ) ;
#4593 = ORIENTED_EDGE ( 'NONE', *, *, #6796, .T. ) ;
#4594 = EDGE_CURVE ( 'NONE', #13601, #19313, #10876, .T. ) ;
#4595 = DIRECTION ( 'NONE',  ( 0.000000000000000000, 0.000000000000000000, 1.000000000000000000 ) ) ;
#4596 = CARTESIAN_POINT ( 'NONE',  ( 0.000000000000000000, 31.88200538760793634, -2.745493118647102548 ) ) ;
#4597 = FACE_OUTER_BOUND ( 'NONE', #12724, .T. ) ;
#4598 = VECTOR ( 'NONE', #18261, 1000.000000000000000 ) ;
#4599 = DIRECTION ( 'NONE',  ( -1.000000000000000000, -0.000000000000000000, -0.000000000000000000 ) ) ;
#4600 = DIRECTION ( 'NONE',  ( 0.000000000000000000, 0.000000000000000000, -1.000000000000000000 ) ) ;
#4601 = UNCERTAINTY_MEASURE_WITH_UNIT (LENGTH_MEASURE( 1.000000000000000082E-05 ), #13982, 'distance_accuracy_value', 'NONE');
#4602 = VERTEX_POINT ( 'NONE', #13135 ) ;
#4603 = CARTESIAN_POINT ( 'NONE',  ( 10.00000000000000000, 6.063030049135491595, -31.42037024962118608 ) ) ;
#4604 = EDGE_CURVE ( 'NONE', #3351, #5871, #17233, .T. ) ;
#4605 = CARTESIAN_POINT ( 'NONE',  ( 10.00000000000000000, -19.83954325428713972, 82.71385593638686373 ) ) ;
#4606 = VERTEX_POINT ( 'NONE', #14690 ) ;
#4607 = EDGE_CURVE ( 'NONE', #10469, #6016, #4181, .T. ) ;
#4608 = FACE_OUTER_BOUND ( 'NONE', #1949, .T. ) ;
#4609 = ORIENTED_EDGE ( 'NONE', *, *, #16020, .T. ) ;
#4610 = DIRECTION ( 'NONE',  ( -1.000000000000000000, -0.000000000000000000, -0.000000000000000000 ) ) ;
#4611 = AXIS2_PLACEMENT_3D ( 'NONE', #13108, #14550, #19967 ) ;
#4612 = FACE_OUTER_BOUND ( 'NONE', #4974, .T. ) ;
#4613 = EDGE_LOOP ( 'NONE', ( #4063, #21833 ) ) ;
#4614 = DIRECTION ( 'NONE',  ( 0.000000000000000000, 0.000000000000000000, -1.000000000000000000 ) ) ;
#4616 = EDGE_CURVE ( 'NONE', #18424, #20435, #310, .T. ) ;
#4615 = ORIENTED_EDGE ( 'NONE', *, *, #18018, .F. ) ;
#4617 = ORIENTED_EDGE ( 'NONE', *, *, #14306, .F. ) ;
#4618 = EDGE_CURVE ( 'NONE', #21664, #12163, #14396, .T. ) ;
#4619 = DIRECTION ( 'NONE',  ( 0.000000000000000000, -0.9271838545667908660, 0.3746065934159030775 ) ) ;
#4620 = VERTEX_POINT ( 'NONE', #3198 ) ;
#4621 = DIRECTION ( 'NONE',  ( 0.000000000000000000, 0.000000000000000000, 1.000000000000000000 ) ) ;
#4622 = EDGE_CURVE ( 'NONE', #18476, #17888, #18124, .T. ) ;
#4623 = VECTOR ( 'NONE', #14869, 1000.000000000000000 ) ;
#4624 = DIRECTION ( 'NONE',  ( 0.000000000000000000, 0.000000000000000000, 1.000000000000000000 ) ) ;
#4625 = DIRECTION ( 'NONE',  ( -1.000000000000000000, 0.000000000000000000, -0.000000000000000000 ) ) ;
#4626 = DIRECTION ( 'NONE',  ( 0.000000000000000000, 0.000000000000000000, 1.000000000000000000 ) ) ;
#4627 = CARTESIAN_POINT ( 'NONE',  ( 10.00000000000000000, 12.46320060045723643, 29.47318494484032314 ) ) ;
#4628 = CARTESIAN_POINT ( 'NONE',  ( 10.00000000000000000, -75.45728100697571961, -39.26051685139143643 ) ) ;
#4629 = DIRECTION ( 'NONE',  ( 0.000000000000000000, 0.000000000000000000, 1.000000000000000000 ) ) ;
#4630 = DIRECTION ( 'NONE',  ( 1.000000000000000000, 0.000000000000000000, 0.000000000000000000 ) ) ;
#4631 = ADVANCED_FACE ( 'NONE', ( #11708 ), #8179, .F. ) ;
#4632 = FACE_OUTER_BOUND ( 'NONE', #968, .T. ) ;
#4633 = EDGE_CURVE ( 'NONE', #20616, #7569, #3837, .T. ) ;
#4634 = CYLINDRICAL_SURFACE ( 'NONE', #5891, 88.00000000000000000 ) ;
#4635 = ORIENTED_EDGE ( 'NONE', *, *, #16480, .T. ) ;
#4636 = EDGE_LOOP ( 'NONE', ( #13059, #9089, #11310, #18154 ) ) ;
#4637 = ADVANCED_FACE ( 'NONE', ( #10040 ), #8398, .F. ) ;
#4638 = ORIENTED_EDGE ( 'NONE', *, *, #13801, .F. ) ;
#4639 = ORIENTED_EDGE ( 'NONE', *, *, #13137, .T. ) ;
#4640 =( GEOMETRIC_REPRESENTATION_CONTEXT ( 3 ) GLOBAL_UNCERTAINTY_ASSIGNED_CONTEXT ( ( #11670 ) ) GLOBAL_UNIT_ASSIGNED_CONTEXT ( ( #16722, #19933, #15724 ) ) REPRESENTATION_CONTEXT ( 'NONE', 'WORKASPACE' ) );
#4641 = VERTEX_POINT ( 'NONE', #10593 ) ;
#4642 = DIRECTION ( 'NONE',  ( 0.000000000000000000, 0.4067366430757947127, 0.9135454576426031981 ) ) ;
#4643 = ADVANCED_FACE ( 'NONE', ( #6967, #15337 ), #5515, .T. ) ;
#4644 = ORIENTED_EDGE ( 'NONE', *, *, #8153, .T. ) ;
#4645 = CYLINDRICAL_SURFACE ( 'NONE', #4676, 88.00000000000000000 ) ;
#4646 = DIRECTION ( 'NONE',  ( 0.000000000000000000, 0.000000000000000000, -1.000000000000000000 ) ) ;
#4647 = DIRECTION ( 'NONE',  ( 1.000000000000000000, 0.000000000000000000, 0.000000000000000000 ) ) ;
#4648 = DIRECTION ( 'NONE',  ( 0.000000000000000000, 0.000000000000000000, 1.000000000000000000 ) ) ;
#4649 = DIRECTION ( 'NONE',  ( -1.000000000000000000, 0.000000000000000000, -0.000000000000000000 ) ) ;
#4650 = DIRECTION ( 'NONE',  ( -1.000000000000000000, 0.000000000000000000, 0.000000000000000000 ) ) ;
#4651 = DIRECTION ( 'NONE',  ( 1.000000000000000000, 0.000000000000000000, 0.000000000000000000 ) ) ;
#4652 = EDGE_LOOP ( 'NONE', ( #20468, #1561, #16123, #11956 ) ) ;
#4653 = DIRECTION ( 'NONE',  ( -1.000000000000000000, -0.000000000000000000, 0.000000000000000000 ) ) ;
#4654 = EDGE_LOOP ( 'NONE', ( #1675, #1836, #12399, #18449 ) ) ;
#4655 = EDGE_CURVE ( 'NONE', #5100, #10149, #9833, .T. ) ;
#4656 = ORIENTED_EDGE ( 'NONE', *, *, #20306, .T. ) ;
#4657 = AXIS2_PLACEMENT_3D ( 'NONE', #1634, #14789, #1516 ) ;
#4658 = CARTESIAN_POINT ( 'NONE',  ( 5.000000000000002665, -87.58454185039434492, -8.540961822682595184 ) ) ;
#4659 = CARTESIAN_POINT ( 'NONE',  ( 0.000000000000000000, -51.10509369859486384, 77.10190917907182495 ) ) ;
#4660 = VERTEX_POINT ( 'NONE', #431 ) ;
#4661 = CARTESIAN_POINT ( 'NONE',  ( 0.000000000000000000, -12.90282758292996235, 25.06465718894773431 ) ) ;
#4662 = ORIENTED_EDGE ( 'NONE', *, *, #6004, .T. ) ;
#4663 = ORIENTED_EDGE ( 'NONE', *, *, #12138, .T. ) ;
#4664 = CARTESIAN_POINT ( 'NONE',  ( 10.00000000000000000, -17.83210509884655792, 21.83428559348755371 ) ) ;
#4665 = ORIENTED_EDGE ( 'NONE', *, *, #9488, .T. ) ;
#4666 = CARTESIAN_POINT ( 'NONE',  ( 0.000000000000000000, 26.27606311335951617, 10.21217444509420424 ) ) ;
#4667 = DIRECTION ( 'NONE',  ( 1.000000000000000000, 0.000000000000000000, 0.000000000000000000 ) ) ;
#4668 = AXIS2_PLACEMENT_3D ( 'NONE', #5544, #13827, #7422 ) ;
#4669 = PLANE ( 'NONE',  #21706 ) ;
#4670 = CARTESIAN_POINT ( 'NONE',  ( 0.000000000000000000, 36.39558101400249512, -80.12091913260344711 ) ) ;
#4671 = FILL_AREA_STYLE ('',( #1254 ) ) ;
#4672 = DIRECTION ( 'NONE',  ( 0.000000000000000000, -0.8660254037844328234, -0.5000000000000101030 ) ) ;
#4673 = DIRECTION ( 'NONE',  ( 0.000000000000000000, 0.000000000000000000, 1.000000000000000000 ) ) ;
#4674 = LINE ( 'NONE', #16500, #18546 ) ;
#4675 = FACE_OUTER_BOUND ( 'NONE', #14571, .T. ) ;
#4676 = AXIS2_PLACEMENT_3D ( 'NONE', #11373, #8074, #18126 ) ;
#4677 = ORIENTED_EDGE ( 'NONE', *, *, #9150, .T. ) ;
#4678 = AXIS2_PLACEMENT_3D ( 'NONE', #1088, #15999, #21305 ) ;
#4679 = ORIENTED_EDGE ( 'NONE', *, *, #2609, .F. ) ;
#4680 = CARTESIAN_POINT ( 'NONE',  ( 10.00000000000000000, -86.66425444033941972, 32.33793443156368852 ) ) ;
#4681 = CARTESIAN_POINT ( 'NONE',  ( 10.00000000000000000, 46.89573839703386682, -79.73220629831438089 ) ) ;
#4682 = CIRCLE ( 'NONE', #17753, 44.99999999999998579 ) ;
#4683 = ORIENTED_EDGE ( 'NONE', *, *, #13285, .T. ) ;
#4684 = CARTESIAN_POINT ( 'NONE',  ( 10.49999999999999822, 1.285879139104720633E-15, 3.000000000000000000 ) ) ;
#4685 = ORIENTED_EDGE ( 'NONE', *, *, #5196, .F. ) ;
#4686 = ADVANCED_FACE ( 'NONE', ( #7289 ), #12245, .F. ) ;
#4687 = VERTEX_POINT ( 'NONE', #3533 ) ;
#4688 = AXIS2_PLACEMENT_3D ( 'NONE', #6539, #16680, #6757 ) ;
#4689 = ORIENTED_EDGE ( 'NONE', *, *, #13797, .F. ) ;
#4690 = ORIENTED_EDGE ( 'NONE', *, *, #11627, .F. ) ;
#4691 = CARTESIAN_POINT ( 'NONE',  ( 10.00000000000000000, -12.90135963484022241, -87.04915231966658951 ) ) ;
#4692 = DIRECTION ( 'NONE',  ( -1.000000000000000000, 0.000000000000000000, -0.000000000000000000 ) ) ;
#4693 = AXIS2_PLACEMENT_3D ( 'NONE', #10307, #15278, #4806 ) ;
#4694 = EDGE_LOOP ( 'NONE', ( #20163, #17216, #11298, #7833 ) ) ;
#4695 = DIRECTION ( 'NONE',  ( 0.000000000000000000, -0.8660254037844432595, 0.4999999999999920064 ) ) ;
#4696 = LINE ( 'NONE', #9886, #7683 ) ;
#4697 = CARTESIAN_POINT ( 'NONE',  ( 10.00000000000000000, 75.27139873020959726, -53.76477968147737840 ) ) ;
#4698 = DIRECTION ( 'NONE',  ( 0.000000000000000000, 0.000000000000000000, 1.000000000000000000 ) ) ;
#4699 = DIRECTION ( 'NONE',  ( 0.000000000000000000, 0.8987940462991680368, -0.4383711467890752389 ) ) ;
#4700 = CARTESIAN_POINT ( 'NONE',  ( 0.000000000000000000, 90.63195040374210976, -18.50093422002330712 ) ) ;
#4701 = VECTOR ( 'NONE', #201, 1000.000000000000000 ) ;
#4702 = VERTEX_POINT ( 'NONE', #5308 ) ;
#4703 = FACE_OUTER_BOUND ( 'NONE', #18858, .T. ) ;
#4704 = VECTOR ( 'NONE', #13094, 1000.000000000000000 ) ;
#4705 = CIRCLE ( 'NONE', #20188, 92.50099999999999056 ) ;
#4706 = DIRECTION ( 'NONE',  ( 1.000000000000000000, 0.000000000000000000, 0.000000000000000000 ) ) ;
#4707 = ADVANCED_FACE ( 'NONE', ( #1866 ), #3858, .F. ) ;
#4708 = ORIENTED_EDGE ( 'NONE', *, *, #13116, .F. ) ;
#4709 = CYLINDRICAL_SURFACE ( 'NONE', #21075, 32.00000000000000000 ) ;
#4710 = ORIENTED_EDGE ( 'NONE', *, *, #5001, .T. ) ;
#4711 = AXIS2_PLACEMENT_3D ( 'NONE', #13167, #18274, #1361 ) ;
#4712 = CARTESIAN_POINT ( 'NONE',  ( 10.00000000000000000, -33.95793648385871677, 86.04239391577979745 ) ) ;
#4713 = DIRECTION ( 'NONE',  ( -1.000000000000000000, -0.000000000000000000, -0.000000000000000000 ) ) ;
#4714 = ORIENTED_EDGE ( 'NONE', *, *, #10117, .F. ) ;
#4715 = EDGE_CURVE ( 'NONE', #3420, #9395, #16554, .T. ) ;
#4716 = DIRECTION ( 'NONE',  ( 0.000000000000000000, -0.6427876096865458022, 0.7660444431189726844 ) ) ;
#4717 = CIRCLE ( 'NONE', #16002, 88.00000000000000000 ) ;
#4718 = ORIENTED_EDGE ( 'NONE', *, *, #18091, .F. ) ;
#4719 = ORIENTED_EDGE ( 'NONE', *, *, #11950, .F. ) ;
#4720 = CARTESIAN_POINT ( 'NONE',  ( -140.0000507999999968, 0.000000000000000000, -1.000000000000000000 ) ) ;
#4721 = EDGE_LOOP ( 'NONE', ( #16674, #15934, #18281, #664 ) ) ;
#4722 = ADVANCED_FACE ( 'NONE', ( #17232 ), #12359, .F. ) ;
#4723 = LINE ( 'NONE', #16763, #2796 ) ;
#4724 = DIRECTION ( 'NONE',  ( 0.000000000000000000, -0.1391731009600517821, -0.9902680687415721383 ) ) ;
#4725 = DIRECTION ( 'NONE',  ( 0.000000000000000000, 0.000000000000000000, 1.000000000000000000 ) ) ;
#4726 = PRODUCT ( 'BR-820', 'BR-820', '', ( #21349 ) ) ;
#4727 = CARTESIAN_POINT ( 'NONE',  ( 10.00000000000000000, -46.93287725819731548, -70.94007663282492615 ) ) ;
#4728 = CIRCLE ( 'NONE', #7915, 88.00000000000000000 ) ;
#4729 = DIRECTION ( 'NONE',  ( 0.000000000000000000, 0.000000000000000000, -1.000000000000000000 ) ) ;
#4730 = CARTESIAN_POINT ( 'NONE',  ( 10.00000000000000000, 0.000000000000000000, 0.000000000000000000 ) ) ;
#4731 = CARTESIAN_POINT ( 'NONE',  ( 10.00000000000000000, -79.38136668499764426, 37.98155635597287016 ) ) ;
#4732 = LINE ( 'NONE', #4526, #8809 ) ;
#4733 = CIRCLE ( 'NONE', #2614, 10.49999999999999822 ) ;
#4734 = EDGE_CURVE ( 'NONE', #5926, #17286, #1378, .T. ) ;
#4735 = CARTESIAN_POINT ( 'NONE',  ( 10.00000000000000000, -80.18694381077088451, -28.37681241246736974 ) ) ;
#4736 = EDGE_CURVE ( 'NONE', #769, #2562, #18886, .T. ) ;
#4737 = EDGE_CURVE ( 'NONE', #10766, #16126, #16901, .T. ) ;
#4738 = DIRECTION ( 'NONE',  ( 0.000000000000000000, 0.000000000000000000, -1.000000000000000000 ) ) ;
#4739 = VECTOR ( 'NONE', #10776, 1000.000000000000000 ) ;
#4740 = ORIENTED_EDGE ( 'NONE', *, *, #12559, .F. ) ;
#4741 = EDGE_CURVE ( 'NONE', #14101, #21516, #7378, .T. ) ;
#4742 = ORIENTED_EDGE ( 'NONE', *, *, #17135, .T. ) ;
#4743 = AXIS2_PLACEMENT_3D ( 'NONE', #3686, #16628, #13304 ) ;
#4744 = ORIENTED_EDGE ( 'NONE', *, *, #456, .F. ) ;
#4745 = VERTEX_POINT ( 'NONE', #8830 ) ;
#4746 = VERTEX_POINT ( 'NONE', #17447 ) ;
#4747 = EDGE_CURVE ( 'NONE', #10528, #9780, #21142, .T. ) ;
#4748 = CARTESIAN_POINT ( 'NONE',  ( 0.000000000000000000, -25.56104204395359503, 81.12843256239655432 ) ) ;
#4749 = AXIS2_PLACEMENT_3D ( 'NONE', #4572, #18054, #2905 ) ;
#4750 = EDGE_LOOP ( 'NONE', ( #14626, #8922, #796, #2137 ) ) ;
#4751 = CARTESIAN_POINT ( 'NONE',  ( -90.00000000000000000, 0.000000000000000000, -7.500000000000020428 ) ) ;
#4752 = CIRCLE ( 'NONE', #10386, 92.50100000000000477 ) ;
#4753 = CARTESIAN_POINT ( 'NONE',  ( 5.000000000000002665, -85.22372865846278955, -21.92979875759713693 ) ) ;
#4754 = ADVANCED_FACE ( 'NONE', ( #18776 ), #103, .F. ) ;
#4755 = CARTESIAN_POINT ( 'NONE',  ( 10.00000000000000000, 0.000000000000000000, 0.000000000000000000 ) ) ;
#4756 = CARTESIAN_POINT ( 'NONE',  ( -10.49999999999999822, 0.000000000000000000, 3.000000000000000000 ) ) ;
#4757 = FILL_AREA_STYLE ('',( #8185 ) ) ;
#4758 = AXIS2_PLACEMENT_3D ( 'NONE', #1190, #2854, #18004 ) ;
#4759 = EDGE_CURVE ( 'NONE', #15531, #13465, #3137, .T. ) ;
#4760 = DIRECTION ( 'NONE',  ( 0.000000000000000000, 0.000000000000000000, 1.000000000000000000 ) ) ;
#4761 = DIRECTION ( 'NONE',  ( 0.000000000000000000, -0.9945218953682742891, 0.1045284632676436315 ) ) ;
#4762 = ORIENTED_EDGE ( 'NONE', *, *, #7302, .F. ) ;
#4763 = CARTESIAN_POINT ( 'NONE',  ( 10.00000000000000000, 0.000000000000000000, 0.000000000000000000 ) ) ;
#4764 = CIRCLE ( 'NONE', #11467, 92.50099999999999056 ) ;
#4765 = EDGE_CURVE ( 'NONE', #6321, #1054, #11615, .T. ) ;
#4766 = AXIS2_PLACEMENT_3D ( 'NONE', #11806, #21746, #1318 ) ;
#4767 = ORIENTED_EDGE ( 'NONE', *, *, #16665, .F. ) ;
#4768 = AXIS2_PLACEMENT_3D ( 'NONE', #19182, #12654, #17977 ) ;
#4769 = ORIENTED_EDGE ( 'NONE', *, *, #4512, .T. ) ;
#4770 = DIRECTION ( 'NONE',  ( 0.000000000000000000, 0.000000000000000000, 1.000000000000000000 ) ) ;
#4771 = ORIENTED_EDGE ( 'NONE', *, *, #15554, .F. ) ;
#4772 = DIRECTION ( 'NONE',  ( 0.000000000000000000, 0.9945218953682737340, -0.1045284632676505149 ) ) ;
#4773 = ORIENTED_EDGE ( 'NONE', *, *, #17566, .F. ) ;
#4774 = ORIENTED_EDGE ( 'NONE', *, *, #6086, .T. ) ;
#4775 = CIRCLE ( 'NONE', #1953, 44.99999999999998579 ) ;
#4776 = ITEM_DEFINED_TRANSFORMATION ( 'NONE', 'NONE', #1465,  #15567 ) ;
#4777 = EDGE_CURVE ( 'NONE', #12008, #10332, #1725, .T. ) ;
#4778 = CARTESIAN_POINT ( 'NONE',  ( 10.00000000000000000, 0.000000000000000000, 0.000000000000000000 ) ) ;
#4779 = EDGE_LOOP ( 'NONE', ( #18375, #1967, #367, #1207 ) ) ;
#4780 = AXIS2_PLACEMENT_3D ( 'NONE', #19941, #11549, #8018 ) ;
#4781 = CYLINDRICAL_SURFACE ( 'NONE', #13934, 88.00000000000000000 ) ;
#4782 = EDGE_CURVE ( 'NONE', #6246, #9931, #17263, .T. ) ;
#4783 = DIRECTION ( 'NONE',  ( -1.000000000000000000, -0.000000000000000000, -0.000000000000000000 ) ) ;
#4784 = FACE_OUTER_BOUND ( 'NONE', #3056, .T. ) ;
#4785 = CARTESIAN_POINT ( 'NONE',  ( -7.440711023145909486, 0.000000000000000000, 0.000000000000000000 ) ) ;
#4786 = AXIS2_PLACEMENT_3D ( 'NONE', #9132, #10787, #10679 ) ;
#4787 = DIRECTION ( 'NONE',  ( 0.000000000000000000, 0.8987940462991680368, -0.4383711467890752389 ) ) ;
#4788 = ADVANCED_FACE ( 'NONE', ( #645 ), #6066, .F. ) ;
#4789 = AXIS2_PLACEMENT_3D ( 'NONE', #8762, #1911, #10629 ) ;
#4790 = CIRCLE ( 'NONE', #16443, 44.99999999999999289 ) ;
#4791 = EDGE_CURVE ( 'NONE', #4066, #6505, #12298, .T. ) ;
#4792 = DIRECTION ( 'NONE',  ( -1.000000000000000000, 0.000000000000000000, -0.000000000000000000 ) ) ;
#4793 = DIRECTION ( 'NONE',  ( -1.000000000000000000, 0.000000000000000000, -0.000000000000000000 ) ) ;
#4795 = CIRCLE ( 'NONE', #19962, 92.50100000000000477 ) ;
#4794 = CYLINDRICAL_SURFACE ( 'NONE', #2753, 45.00000000000000000 ) ;
#4796 = ORIENTED_EDGE ( 'NONE', *, *, #128, .T. ) ;
#4797 = CARTESIAN_POINT ( 'NONE',  ( -120.0000000000000000, 1.469576158976823671E-14, -3.000000000000000000 ) ) ;
#4798 = CARTESIAN_POINT ( 'NONE',  ( 10.00000000000000000, 14.53731623274928708, 23.34226719384910709 ) ) ;
#4799 = VERTEX_POINT ( 'NONE', #21195 ) ;
#4800 = AXIS2_PLACEMENT_3D ( 'NONE', #8567, #11993, #20899 ) ;
#4801 = CARTESIAN_POINT ( 'NONE',  ( 10.00000000000000000, -46.93287725819829603, 70.94007663282431508 ) ) ;
#4802 = AXIS2_PLACEMENT_3D ( 'NONE', #10980, #9419, #17954 ) ;
#4803 = ORIENTED_EDGE ( 'NONE', *, *, #1939, .F. ) ;
#4804 = CIRCLE ( 'NONE', #8683, 44.99999999999999289 ) ;
#4805 = ORIENTED_EDGE ( 'NONE', *, *, #2439, .F. ) ;
#4806 = DIRECTION ( 'NONE',  ( 0.000000000000000000, -0.8987940462991618196, -0.4383711467890877289 ) ) ;
#4807 = EDGE_LOOP ( 'NONE', ( #6388, #242, #531, #6959 ) ) ;
#4808 = ORIENTED_EDGE ( 'NONE', *, *, #2528, .F. ) ;
#4809 = CARTESIAN_POINT ( 'NONE',  ( -90.00000000000000000, 0.000000000000000000, -6.887500000000022382 ) ) ;
#4810 = DIRECTION ( 'NONE',  ( 0.000000000000000000, 0.4694715627858855322, 0.8829475928589297640 ) ) ;
#4811 = VERTEX_POINT ( 'NONE', #9146 ) ;
#4812 = DIRECTION ( 'NONE',  ( 0.000000000000000000, 0.000000000000000000, 1.000000000000000000 ) ) ;
#4813 = DIRECTION ( 'NONE',  ( 1.000000000000000000, 0.000000000000000000, 0.000000000000000000 ) ) ;
#4814 = DIRECTION ( 'NONE',  ( 0.000000000000000000, 0.000000000000000000, -1.000000000000000000 ) ) ;
#4815 = CARTESIAN_POINT ( 'NONE',  ( 10.00000000000000000, -27.87320266523496315, -88.20158487341788600 ) ) ;
#4816 = FACE_OUTER_BOUND ( 'NONE', #9999, .T. ) ;
#4817 = DIRECTION ( 'NONE',  ( 1.000000000000000000, -0.000000000000000000, -0.000000000000000000 ) ) ;
#4818 = UNCERTAINTY_MEASURE_WITH_UNIT (LENGTH_MEASURE( 1.000000000000000082E-05 ), #2589, 'distance_accuracy_value', 'NONE');
#4819 = CIRCLE ( 'NONE', #20684, 88.00000000000000000 ) ;
#4820 = ORIENTED_EDGE ( 'NONE', *, *, #12687, .F. ) ;
#4821 = AXIS2_PLACEMENT_3D ( 'NONE', #16469, #21656, #16250 ) ;
#4822 = CIRCLE ( 'NONE', #13119, 92.50099999999999056 ) ;
#4823 = DIRECTION ( 'NONE',  ( 0.000000000000000000, 0.000000000000000000, -1.000000000000000000 ) ) ;
#4824 = FACE_OUTER_BOUND ( 'NONE', #10229, .T. ) ;
#4825 = ORIENTED_EDGE ( 'NONE', *, *, #712, .T. ) ;
#4826 = DIRECTION ( 'NONE',  ( -1.000000000000000000, 0.000000000000000000, 0.000000000000000000 ) ) ;
#4827 = ORIENTED_EDGE ( 'NONE', *, *, #1345, .T. ) ;
#4828 = DIRECTION ( 'NONE',  ( 0.000000000000000000, 0.000000000000000000, 1.000000000000000000 ) ) ;
#4829 = CARTESIAN_POINT ( 'NONE',  ( 10.00000000000000000, 0.000000000000000000, 0.000000000000000000 ) ) ;
#4830 = ORIENTED_EDGE ( 'NONE', *, *, #831, .T. ) ;
#4831 = CARTESIAN_POINT ( 'NONE',  ( 0.000000000000000000, -64.66851233300690183, -55.25552418573029456 ) ) ;
#4832 = VECTOR ( 'NONE', #16253, 1000.000000000000000 ) ;
#4833 = EDGE_LOOP ( 'NONE', ( #5985, #20046, #6965, #4969 ) ) ;
#4834 = AXIS2_PLACEMENT_3D ( 'NONE', #19659, #19539, #2863 ) ;
#4835 = ORIENTED_EDGE ( 'NONE', *, *, #14481, .F. ) ;
#4836 = DIRECTION ( 'NONE',  ( 0.000000000000000000, 0.000000000000000000, 1.000000000000000000 ) ) ;
#4837 = VECTOR ( 'NONE', #4521, 1000.000000000000000 ) ;
#4838 = ORIENTED_EDGE ( 'NONE', *, *, #20951, .F. ) ;
#4839 = CARTESIAN_POINT ( 'NONE',  ( 5.000000000000000000, 47.19205848891868271, -74.27590198428072199 ) ) ;
#4840 = CARTESIAN_POINT ( 'NONE',  ( -90.00000000000000000, 8.434754829127421589E-16, 6.887500000000022382 ) ) ;
#4841 = CARTESIAN_POINT ( 'NONE',  ( -1.139999999999998570, 0.000000000000000000, 0.000000000000000000 ) ) ;
#4842 = ADVANCED_FACE ( 'NONE', ( #17666 ), #4283, .T. ) ;
#4843 = DIRECTION ( 'NONE',  ( -1.000000000000000000, -0.000000000000000000, -0.000000000000000000 ) ) ;
#4844 = FILL_AREA_STYLE_COLOUR ( '', #20928 ) ;
#4845 = DIRECTION ( 'NONE',  ( 1.000000000000000000, 0.000000000000000000, 0.000000000000000000 ) ) ;
#4846 = DIRECTION ( 'NONE',  ( 0.000000000000000000, 0.000000000000000000, 1.000000000000000000 ) ) ;
#4847 = EDGE_CURVE ( 'NONE', #20877, #13006, #859, .T. ) ;
#4848 = LINE ( 'NONE', #11590, #19374 ) ;
#4849 = CIRCLE ( 'NONE', #15785, 92.50100000000003320 ) ;
#4850 = CARTESIAN_POINT ( 'NONE',  ( 0.000000000000000000, -81.34229909304657724, -33.57723005635448743 ) ) ;
#4851 = VECTOR ( 'NONE', #14439, 1000.000000000000000 ) ;
#4852 = CIRCLE ( 'NONE', #278, 88.00000000000000000 ) ;
#4853 = DIRECTION ( 'NONE',  ( -1.000000000000000000, -0.000000000000000000, -0.000000000000000000 ) ) ;
#4854 = ORIENTED_EDGE ( 'NONE', *, *, #13738, .F. ) ;
#4855 = ORIENTED_EDGE ( 'NONE', *, *, #991, .F. ) ;
#4856 = ORIENTED_EDGE ( 'NONE', *, *, #8828, .T. ) ;
#4857 = ORIENTED_EDGE ( 'NONE', *, *, #13644, .T. ) ;
#4858 = VERTEX_POINT ( 'NONE', #4069 ) ;
#4859 = CARTESIAN_POINT ( 'NONE',  ( 10.00000000000000000, -41.89587599971492438, -77.38692120905515992 ) ) ;
#4860 = AXIS2_PLACEMENT_3D ( 'NONE', #12427, #4482, #21170 ) ;
#4861 = VERTEX_POINT ( 'NONE', #17556 ) ;
#4862 = DIRECTION ( 'NONE',  ( 1.000000000000000000, 0.000000000000000000, 0.000000000000000000 ) ) ;
#4863 = ADVANCED_FACE ( 'NONE', ( #7820 ), #753, .T. ) ;
#4864 = CIRCLE ( 'NONE', #16848, 44.99999999999999289 ) ;
#4865 = EDGE_CURVE ( 'NONE', #17077, #1435, #7719, .T. ) ;
#4866 = EDGE_CURVE ( 'NONE', #3210, #5078, #14065, .T. ) ;
#4867 = CIRCLE ( 'NONE', #14382, 88.00000000000000000 ) ;
#4868 = DIRECTION ( 'NONE',  ( -1.000000000000000000, 0.000000000000000000, 0.000000000000000000 ) ) ;
#4869 = EDGE_CURVE ( 'NONE', #4687, #11658, #12680, .T. ) ;
#4870 = DIRECTION ( 'NONE',  ( -1.000000000000000000, -0.000000000000000000, -0.000000000000000000 ) ) ;
#4871 = FACE_OUTER_BOUND ( 'NONE', #10991, .T. ) ;
#4872 = DIRECTION ( 'NONE',  ( -0.000000000000000000, -0.000000000000000000, 1.000000000000000000 ) ) ;
#4873 = LINE ( 'NONE', #19675, #1662 ) ;
#4874 = CIRCLE ( 'NONE', #3812, 45.00000000000000711 ) ;
#4875 = DIRECTION ( 'NONE',  ( -1.000000000000000000, 0.000000000000000000, -0.000000000000000000 ) ) ;
#4876 = VERTEX_POINT ( 'NONE', #14343 ) ;
#4877 = CARTESIAN_POINT ( 'NONE',  ( 5.000000000000000000, 57.06999622551897033, -66.98518889142023625 ) ) ;
#4878 = EDGE_CURVE ( 'NONE', #2527, #19897, #20070, .T. ) ;
#4879 = AXIS2_PLACEMENT_3D ( 'NONE', #20115, #18355, #4642 ) ;
#4880 = VECTOR ( 'NONE', #15733, 1000.000000000000000 ) ;
#4881 = ORIENTED_EDGE ( 'NONE', *, *, #15035, .T. ) ;
#4882 = CIRCLE ( 'NONE', #19338, 44.99999999999999289 ) ;
#4883 = ORIENTED_EDGE ( 'NONE', *, *, #21501, .F. ) ;
#4884 = EDGE_CURVE ( 'NONE', #7563, #508, #7030, .T. ) ;
#4885 = CARTESIAN_POINT ( 'NONE',  ( 0.000000000000000000, 0.000000000000000000, 0.000000000000000000 ) ) ;
#4886 = VERTEX_POINT ( 'NONE', #10916 ) ;
#4887 = CARTESIAN_POINT ( 'NONE',  ( 0.000000000000000000, 48.19312842678564834, -70.09002648625148879 ) ) ;
#4888 = ORIENTED_EDGE ( 'NONE', *, *, #5449, .F. ) ;
#4889 = VERTEX_POINT ( 'NONE', #12456 ) ;
#4890 = CARTESIAN_POINT ( 'NONE',  ( 10.00000000000000000, -2.481790431838652111, -92.46770094066596357 ) ) ;
#4891 = ORIENTED_EDGE ( 'NONE', *, *, #4086, .T. ) ;
#4892 = CARTESIAN_POINT ( 'NONE',  ( 10.00000000000000000, 0.000000000000000000, 0.000000000000000000 ) ) ;
#4893 = CARTESIAN_POINT ( 'NONE',  ( 9.999999999999996447, 1.238117913937974620E-14, 101.1000000000000512 ) ) ;
#4894 = EDGE_CURVE ( 'NONE', #15140, #21168, #2626, .T. ) ;
#4895 = CARTESIAN_POINT ( 'NONE',  ( 5.000000000000000000, -36.39558101400082535, -80.12091913260421450 ) ) ;
#4896 = FACE_OUTER_BOUND ( 'NONE', #4493, .T. ) ;
#4897 = CIRCLE ( 'NONE', #21472, 3.000000000000000444 ) ;
#4898 = CARTESIAN_POINT ( 'NONE',  ( 10.00000000000000000, 23.62010150527222052, 84.77081340225913664 ) ) ;
#4899 = VECTOR ( 'NONE', #16580, 1000.000000000000000 ) ;
#4900 = VECTOR ( 'NONE', #19253, 1000.000000000000000 ) ;
#4901 = CIRCLE ( 'NONE', #18663, 45.00000000000000000 ) ;
#4902 = DIRECTION ( 'NONE',  ( 0.000000000000000000, 0.000000000000000000, -1.000000000000000000 ) ) ;
#4903 = DIRECTION ( 'NONE',  ( -1.000000000000000000, 0.000000000000000000, 0.000000000000000000 ) ) ;
#4904 = CARTESIAN_POINT ( 'NONE',  ( 0.000000000000000000, -76.53853822674008711, 43.42639941457088781 ) ) ;
#4905 = ORIENTED_EDGE ( 'NONE', *, *, #20306, .F. ) ;
#4906 = EDGE_CURVE ( 'NONE', #1686, #1185, #21297, .T. ) ;
#4907 = CIRCLE ( 'NONE', #12655, 44.99999999999998579 ) ;
#4908 = ADVANCED_FACE ( 'NONE', ( #972 ), #19527, .F. ) ;
#4909 = DIRECTION ( 'NONE',  ( 0.000000000000000000, 0.000000000000000000, -1.000000000000000000 ) ) ;
#4910 = VECTOR ( 'NONE', #16109, 1000.000000000000000 ) ;
#4911 = DIRECTION ( 'NONE',  ( 1.000000000000000000, -0.000000000000000000, -0.000000000000000000 ) ) ;
#4912 = VERTEX_POINT ( 'NONE', #4180 ) ;
#4913 = CIRCLE ( 'NONE', #10896, 92.50100000000000477 ) ;
#4914 = EDGE_CURVE ( 'NONE', #18417, #16952, #10188, .T. ) ;
#4915 = AXIS2_PLACEMENT_3D ( 'NONE', #13684, #20436, #17110 ) ;
#4916 = DIRECTION ( 'NONE',  ( 0.000000000000000000, 0.000000000000000000, -1.000000000000000000 ) ) ;
#4918 = AXIS2_PLACEMENT_3D ( 'NONE', #12146, #10491, #20658 ) ;
#4917 = PRODUCT_DEFINITION_SHAPE ( 'NONE', 'NONE',  #4011 ) ;
#4919 = ORIENTED_EDGE ( 'NONE', *, *, #4096, .T. ) ;
#4920 = ADVANCED_FACE ( 'NONE', ( #14555 ), #12899, .T. ) ;
#4921 = ORIENTED_EDGE ( 'NONE', *, *, #8271, .T. ) ;
#4922 = CARTESIAN_POINT ( 'NONE',  ( 1.500000000000000888, 6.245698675651501825E-16, 5.100000000000000533 ) ) ;
#4923 = ORIENTED_EDGE ( 'NONE', *, *, #17207, .T. ) ;
#4924 = EDGE_LOOP ( 'NONE', ( #21070, #16187, #10783, #4638 ) ) ;
#4925 = CARTESIAN_POINT ( 'NONE',  ( 0.000000000000000000, -85.54350296776095774, -20.64725405482940346 ) ) ;
#4926 = VERTEX_POINT ( 'NONE', #3182 ) ;
#4927 = ORIENTED_EDGE ( 'NONE', *, *, #9577, .T. ) ;
#4928 = EDGE_CURVE ( 'NONE', #14192, #2555, #15485, .T. ) ;
#4929 = FACE_OUTER_BOUND ( 'NONE', #5475, .T. ) ;
#4930 = DIRECTION ( 'NONE',  ( -1.000000000000000000, -0.000000000000000000, -0.000000000000000000 ) ) ;
#4931 = FACE_OUTER_BOUND ( 'NONE', #20528, .T. ) ;
#4932 = CARTESIAN_POINT ( 'NONE',  ( 10.00000000000000000, 0.000000000000000000, 0.000000000000000000 ) ) ;
#4933 = DIRECTION ( 'NONE',  ( 1.000000000000000000, 0.000000000000000000, 0.000000000000000000 ) ) ;
#4934 = DIRECTION ( 'NONE',  ( 0.000000000000000000, -0.4694715627858798146, -0.8829475928589327616 ) ) ;
#4935 = CIRCLE ( 'NONE', #1025, 11.99999999999999822 ) ;
#4936 = VECTOR ( 'NONE', #19718, 1000.000000000000000 ) ;
#4937 = COLOUR_RGB ( '', 0.09019608, 0.27058824, 0.51372549) ;
#4938 = ORIENTED_EDGE ( 'NONE', *, *, #20938, .F. ) ;
#4939 = AXIS2_PLACEMENT_3D ( 'NONE', #520, #15976, #10901 ) ;
#4940 = LINE ( 'NONE', #14973, #5303 ) ;
#4941 = DIRECTION ( 'NONE',  ( -1.000000000000000000, 0.000000000000000000, 0.000000000000000000 ) ) ;
#4942 = EDGE_LOOP ( 'NONE', ( #13003, #11622, #9695, #4413 ) ) ;
#4943 = CARTESIAN_POINT ( 'NONE',  ( 0.000000000000000000, 12.90282758293013643, -25.06465718894764194 ) ) ;
#4944 = ORIENTED_EDGE ( 'NONE', *, *, #969, .T. ) ;
#4945 = CARTESIAN_POINT ( 'NONE',  ( 10.00000000000000000, -7.409634587003275819, 27.19958299168154880 ) ) ;
#4946 = CARTESIAN_POINT ( 'NONE',  ( 0.000000000000000000, 0.000000000000000000, 25.00000000000000000 ) ) ;
#4947 = ORIENTED_EDGE ( 'NONE', *, *, #2788, .F. ) ;
#4948 = CARTESIAN_POINT ( 'NONE',  ( 10.00000000000000000, -27.07404830566974141, 4.815694066514342175 ) ) ;
#4949 = EDGE_LOOP ( 'NONE', ( #7138, #316, #5329, #16978, #14225 ) ) ;
#4950 = ORIENTED_EDGE ( 'NONE', *, *, #11770, .T. ) ;
#4951 = AXIS2_PLACEMENT_3D ( 'NONE', #20483, #2232, #2024 ) ;
#4952 = DIRECTION ( 'NONE',  ( 0.000000000000000000, -0.6946583704589885944, -0.7193398003386594075 ) ) ;
#4953 = ORIENTED_EDGE ( 'NONE', *, *, #5987, .F. ) ;
#4954 = FACE_OUTER_BOUND ( 'NONE', #19775, .T. ) ;
#4955 = CARTESIAN_POINT ( 'NONE',  ( 0.000000000000000000, 0.000000000000000000, 0.000000000000000000 ) ) ;
#4956 = DIRECTION ( 'NONE',  ( -1.000000000000000000, -0.000000000000000000, 0.000000000000000000 ) ) ;
#4957 = CARTESIAN_POINT ( 'NONE',  ( 5.000000000000002665, -76.53853822674008711, 43.42639941457088781 ) ) ;
#4958 = DIRECTION ( 'NONE',  ( 1.000000000000000000, 0.000000000000000000, 0.000000000000000000 ) ) ;
#4959 = CARTESIAN_POINT ( 'NONE',  ( 10.00000000000000000, 0.000000000000000000, 0.000000000000000000 ) ) ;
#4960 = DIRECTION ( 'NONE',  ( -1.000000000000000000, -0.000000000000000000, -0.000000000000000000 ) ) ;
#4961 = FACE_OUTER_BOUND ( 'NONE', #12921, .T. ) ;
#4962 = CARTESIAN_POINT ( 'NONE',  ( 9.999999999999980460, 0.000000000000000000, 0.000000000000000000 ) ) ;
#4963 = AXIS2_PLACEMENT_3D ( 'NONE', #8968, #18930, #585 ) ;
#4964 = CARTESIAN_POINT ( 'NONE',  ( 10.00000000000000000, 0.000000000000000000, 0.000000000000000000 ) ) ;
#4965 = VERTEX_POINT ( 'NONE', #16553 ) ;
#4966 = CARTESIAN_POINT ( 'NONE',  ( 10.00000000000000000, -24.73395913766455578, -12.01774797440602427 ) ) ;
#4967 = EDGE_CURVE ( 'NONE', #21786, #15480, #11262, .T. ) ;
#4968 = ORIENTED_EDGE ( 'NONE', *, *, #9054, .F. ) ;
#4969 = ORIENTED_EDGE ( 'NONE', *, *, #14359, .T. ) ;
#4970 = VERTEX_POINT ( 'NONE', #14667 ) ;
#4971 = EDGE_CURVE ( 'NONE', #17333, #7568, #20456, .T. ) ;
#4972 = ORIENTED_EDGE ( 'NONE', *, *, #10099, .F. ) ;
#4973 = DIRECTION ( 'NONE',  ( -1.000000000000000000, 0.000000000000000000, 0.000000000000000000 ) ) ;
#4974 = EDGE_LOOP ( 'NONE', ( #13444, #1755, #21066, #12056 ) ) ;
#4975 = FACE_OUTER_BOUND ( 'NONE', #15482, .T. ) ;
#4976 = AXIS2_PLACEMENT_3D ( 'NONE', #13004, #4506, #3062 ) ;
#4977 = CARTESIAN_POINT ( 'NONE',  ( 10.00000000000000000, 0.000000000000000000, 0.000000000000000000 ) ) ;
#4978 = DIRECTION ( 'NONE',  ( 0.000000000000000000, 0.000000000000000000, 1.000000000000000000 ) ) ;
#4979 = DIRECTION ( 'NONE',  ( 0.000000000000000000, 0.000000000000000000, 1.000000000000000000 ) ) ;
#4980 = DIRECTION ( 'NONE',  ( 1.000000000000000000, 0.000000000000000000, 0.000000000000000000 ) ) ;
#4981 = LINE ( 'NONE', #11502, #7702 ) ;
#4982 = VERTEX_POINT ( 'NONE', #9567 ) ;
#4983 = DIRECTION ( 'NONE',  ( -1.000000000000000000, -0.000000000000000000, -0.000000000000000000 ) ) ;
#4984 = ADVANCED_FACE ( 'NONE', ( #11347 ), #21624, .F. ) ;
#4985 = ORIENTED_EDGE ( 'NONE', *, *, #4971, .F. ) ;
#4986 = ORIENTED_EDGE ( 'NONE', *, *, #716, .T. ) ;
#4987 = CARTESIAN_POINT ( 'NONE',  ( 1.500000000000001332, 0.000000000000000000, 5.453125000000000000 ) ) ;
#4988 = VERTEX_POINT ( 'NONE', #8260 ) ;
#4989 = DIRECTION ( 'NONE',  ( -1.000000000000000000, -0.000000000000000000, 0.000000000000000000 ) ) ;
#4990 = VERTEX_POINT ( 'NONE', #20089 ) ;
#4991 = ORIENTED_EDGE ( 'NONE', *, *, #851, .F. ) ;
#4992 = PRODUCT_CONTEXT ( 'NONE', #1204, 'mechanical' ) ;
#4993 = DIRECTION ( 'NONE',  ( 0.000000000000000000, 0.000000000000000000, 1.000000000000000000 ) ) ;
#4994 = ORIENTED_EDGE ( 'NONE', *, *, #1618, .F. ) ;
#4995 = CARTESIAN_POINT ( 'NONE',  ( 10.00000000000000000, 0.6021240089801420670, 31.99433460282944708 ) ) ;
#4996 = ADVANCED_FACE ( 'NONE', ( #11689 ), #21413, .T. ) ;
#4997 = CARTESIAN_POINT ( 'NONE',  ( 10.00000000000000000, 61.60362715319122628, -62.84101464466179721 ) ) ;
#4998 = DIRECTION ( 'NONE',  ( 0.000000000000000000, 0.4067366430758010964, -0.9135454576426006446 ) ) ;
#4999 = COLOUR_RGB ( '', 0.66274510, 0.83137255, 0.94901961) ;
#5000 = DIRECTION ( 'NONE',  ( -1.000000000000000000, 0.000000000000000000, 0.000000000000000000 ) ) ;
#5001 = EDGE_CURVE ( 'NONE', #4259, #14855, #18098, .T. ) ;
#5002 = CARTESIAN_POINT ( 'NONE',  ( 10.00000000000000000, -9.992993448021419312, -26.36019881529895770 ) ) ;
#5003 = CARTESIAN_POINT ( 'NONE',  ( 10.00000000000000000, -64.66851233300764079, 55.25552418572942059 ) ) ;
#5004 = ORIENTED_EDGE ( 'NONE', *, *, #3956, .F. ) ;
#5005 = EDGE_CURVE ( 'NONE', #7352, #19098, #4723, .T. ) ;
#5006 = EDGE_CURVE ( 'NONE', #11182, #11054, #6406, .T. ) ;
#5007 = ADVANCED_FACE ( 'NONE', ( #4954 ), #6294, .F. ) ;
#5008 = CARTESIAN_POINT ( 'NONE',  ( 10.00000000000000000, 0.000000000000000000, 0.000000000000000000 ) ) ;
#5009 =( REPRESENTATION_RELATIONSHIP ('NONE','NONE', #2177, #6721 ) REPRESENTATION_RELATIONSHIP_WITH_TRANSFORMATION ( #8097 )SHAPE_REPRESENTATION_RELATIONSHIP( ) );
#5010 = ADVANCED_FACE ( 'NONE', ( #14994 ), #18331, .F. ) ;
#5011 = DIRECTION ( 'NONE',  ( 1.000000000000000000, 0.000000000000000000, 0.000000000000000000 ) ) ;
#5012 = EDGE_LOOP ( 'NONE', ( #3495, #13267, #15775, #2234 ) ) ;
#5013 = CARTESIAN_POINT ( 'NONE',  ( 0.000000000000000000, 84.80486432185243473, -36.94008646920313055 ) ) ;
#5014 = ORIENTED_EDGE ( 'NONE', *, *, #15695, .F. ) ;
#5015 =( NAMED_UNIT ( * ) PLANE_ANGLE_UNIT ( ) SI_UNIT ( $, .RADIAN. ) );
#5016 = EDGE_LOOP ( 'NONE', ( #3219, #12191, #15836, #7510 ) ) ;
#5017 = DIRECTION ( 'NONE',  ( -0.000000000000000000, 0.000000000000000000, -1.000000000000000000 ) ) ;
#5018 = VECTOR ( 'NONE', #21574, 1000.000000000000000 ) ;
#5019 = ORIENTED_EDGE ( 'NONE', *, *, #4734, .F. ) ;
#5020 = ORIENTED_EDGE ( 'NONE', *, *, #18910, .T. ) ;
#5021 = DIRECTION ( 'NONE',  ( 0.000000000000000000, -1.000000000000000000, 0.000000000000000000 ) ) ;
#5022 = DIRECTION ( 'NONE',  ( 0.000000000000000000, 0.000000000000000000, -1.000000000000000000 ) ) ;
#5023 = EDGE_LOOP ( 'NONE', ( #1078, #4679, #10655, #17133 ) ) ;
#5024 = EDGE_CURVE ( 'NONE', #4316, #15667, #21159, .T. ) ;
#5025 = AXIS2_PLACEMENT_3D ( 'NONE', #2033, #13634, #20386 ) ;
#5026 = DIRECTION ( 'NONE',  ( -1.000000000000000000, -0.000000000000000000, 0.000000000000000000 ) ) ;
#5027 = CARTESIAN_POINT ( 'NONE',  ( 10.00000000000000000, -7.619321854369744074, 26.42235673590688094 ) ) ;
#5028 = LINE ( 'NONE', #8346, #11852 ) ;
#5029 = DIRECTION ( 'NONE',  ( 1.000000000000000000, 0.000000000000000000, 0.000000000000000000 ) ) ;
#5030 = FACE_OUTER_BOUND ( 'NONE', #14932, .T. ) ;
#5031 = EDGE_CURVE ( 'NONE', #21500, #5074, #1400, .T. ) ;
#5032 = CARTESIAN_POINT ( 'NONE',  ( 10.00000000000000000, -91.49386717542212466, -13.61276130277086693 ) ) ;
#5033 = ORIENTED_EDGE ( 'NONE', *, *, #16809, .T. ) ;
#5034 = ADVANCED_FACE ( 'NONE', ( #6733 ), #13335, .T. ) ;
#5035 = DIRECTION ( 'NONE',  ( -1.000000000000000000, -0.000000000000000000, 0.000000000000000000 ) ) ;
#5036 = AXIS2_PLACEMENT_3D ( 'NONE', #1545, #9709, #11608 ) ;
#5037 = CYLINDRICAL_SURFACE ( 'NONE', #17153, 104.9000000000000341 ) ;
#5038 = ORIENTED_EDGE ( 'NONE', *, *, #16407, .F. ) ;
#5039 = CARTESIAN_POINT ( 'NONE',  ( 5.000000000000000000, -60.65279801375385915, 63.75921967137595914 ) ) ;
#5040 = ORIENTED_EDGE ( 'NONE', *, *, #17566, .T. ) ;
#5041 = AXIS2_PLACEMENT_3D ( 'NONE', #6431, #6094, #18028 ) ;
#5042 = EDGE_CURVE ( 'NONE', #11544, #20880, #3284, .T. ) ;
#5043 = SURFACE_STYLE_USAGE ( .BOTH. , #13323 ) ;
#5044 = DIRECTION ( 'NONE',  ( -1.000000000000000000, -0.000000000000000000, -0.000000000000000000 ) ) ;
#5045 = ORIENTED_EDGE ( 'NONE', *, *, #7645, .F. ) ;
#5046 = AXIS2_PLACEMENT_3D ( 'NONE', #5609, #12230, #7267 ) ;
#5047 = DIRECTION ( 'NONE',  ( -1.000000000000000000, 0.000000000000000000, 0.000000000000000000 ) ) ;
#5048 = ADVANCED_FACE ( 'NONE', ( #3070 ), #2853, .T. ) ;
#5049 = VERTEX_POINT ( 'NONE', #15430 ) ;
#5050 = AXIS2_PLACEMENT_3D ( 'NONE', #19347, #4213, #9271 ) ;
#5051 = VERTEX_POINT ( 'NONE', #13555 ) ;
#5052 = ORIENTED_EDGE ( 'NONE', *, *, #21568, .T. ) ;
#5053 = DIRECTION ( 'NONE',  ( -0.000000000000000000, 0.000000000000000000, -1.000000000000000000 ) ) ;
#5054 = EDGE_LOOP ( 'NONE', ( #5784, #16281, #10069, #3462 ) ) ;
#5055 = CARTESIAN_POINT ( 'NONE',  ( -1.500000000000000000, 0.000000000000000000, 15.00000000000000000 ) ) ;
#5056 = AXIS2_PLACEMENT_3D ( 'NONE', #21301, #4518, #2856 ) ;
#5057 = CARTESIAN_POINT ( 'NONE',  ( 10.00000000000000000, 0.000000000000000000, 0.000000000000000000 ) ) ;
#5058 = CARTESIAN_POINT ( 'NONE',  ( 10.00000000000000000, 0.000000000000000000, 0.000000000000000000 ) ) ;
#5059 = DIRECTION ( 'NONE',  ( -1.000000000000000000, -0.000000000000000000, -0.000000000000000000 ) ) ;
#5060 = EDGE_CURVE ( 'NONE', #6638, #935, #10548, .T. ) ;
#5061 = CARTESIAN_POINT ( 'NONE',  ( 0.000000000000000000, 31.15801000616942673, -79.14775961996359399 ) ) ;
#5062 = VECTOR ( 'NONE', #12088, 1000.000000000000000 ) ;
#5063 = AXIS2_PLACEMENT_3D ( 'NONE', #14996, #16556, #21846 ) ;
#5064 = DIRECTION ( 'NONE',  ( -1.000000000000000000, 0.000000000000000000, 0.000000000000000000 ) ) ;
#5065 = CYLINDRICAL_SURFACE ( 'NONE', #12087, 88.00000000000000000 ) ;
#5066 = AXIS2_PLACEMENT_3D ( 'NONE', #16957, #3472, #1708 ) ;
#5067 = EDGE_CURVE ( 'NONE', #13354, #14952, #21844, .T. ) ;
#5068 = CYLINDRICAL_SURFACE ( 'NONE', #13032, 11.99999999999999645 ) ;
#5069 = CYLINDRICAL_SURFACE ( 'NONE', #4766, 44.99999999999999289 ) ;
#5070 = DIRECTION ( 'NONE',  ( 0.000000000000000000, 0.9993908270190955401, 0.03489949670250440394 ) ) ;
#5071 = ORIENTED_EDGE ( 'NONE', *, *, #3565, .F. ) ;
#5072 = AXIS2_PLACEMENT_3D ( 'NONE', #4727, #1747, #2957 ) ;
#5073 = CARTESIAN_POINT ( 'NONE',  ( 5.000000000000002665, 40.72878876293257377, -78.00747250042405767 ) ) ;
#5074 = VERTEX_POINT ( 'NONE', #20309 ) ;
#5075 = DIRECTION ( 'NONE',  ( 0.000000000000000000, 0.000000000000000000, 1.000000000000000000 ) ) ;
#5076 = ORIENTED_EDGE ( 'NONE', *, *, #1198, .T. ) ;
#5077 = AXIS2_PLACEMENT_3D ( 'NONE', #13615, #364, #20368 ) ;
#5078 = VERTEX_POINT ( 'NONE', #10130 ) ;
#5079 = AXIS2_PLACEMENT_3D ( 'NONE', #12946, #7987, #1244 ) ;
#5080 = ORIENTED_EDGE ( 'NONE', *, *, #15907, .T. ) ;
#5081 = DIRECTION ( 'NONE',  ( -1.000000000000000000, 0.000000000000000000, 0.000000000000000000 ) ) ;
#5082 = ORIENTED_EDGE ( 'NONE', *, *, #9306, .F. ) ;
#5083 = FACE_OUTER_BOUND ( 'NONE', #1147, .T. ) ;
#5084 = CARTESIAN_POINT ( 'NONE',  ( 10.00000000000000000, 66.01871308925461790, 64.79170103523043167 ) ) ;
#5085 = VECTOR ( 'NONE', #19082, 1000.000000000000000 ) ;
#5086 = DIRECTION ( 'NONE',  ( -1.000000000000000000, -0.000000000000000000, -0.000000000000000000 ) ) ;
#5087 = LINE ( 'NONE', #15234, #15059 ) ;
#5088 = CARTESIAN_POINT ( 'NONE',  ( 0.000000000000000000, 0.000000000000000000, 0.000000000000000000 ) ) ;
#5089 = DIRECTION ( 'NONE',  ( 0.000000000000000000, 0.000000000000000000, 1.000000000000000000 ) ) ;
#5090 = CARTESIAN_POINT ( 'NONE',  ( 0.000000000000000000, 0.000000000000000000, -3.000000000000000000 ) ) ;
#5091 = VECTOR ( 'NONE', #9546, 1000.000000000000000 ) ;
#5092 = ORIENTED_EDGE ( 'NONE', *, *, #5910, .F. ) ;
#5093 = CIRCLE ( 'NONE', #1900, 12.00000000000000000 ) ;
#5094 = ADVANCED_BREP_SHAPE_REPRESENTATION ( '', ( #6054, #15567 ), #3229 ) ;
#5095 = DIRECTION ( 'NONE',  ( 1.000000000000000000, 0.000000000000000000, 0.000000000000000000 ) ) ;
#5096 = ORIENTED_EDGE ( 'NONE', *, *, #8486, .T. ) ;
#5097 = VERTEX_POINT ( 'NONE', #20419 ) ;
#5098 = DIRECTION ( 'NONE',  ( -1.000000000000000000, 0.000000000000000000, 0.000000000000000000 ) ) ;
#5099 = VECTOR ( 'NONE', #15400, 1000.000000000000000 ) ;
#5100 = VERTEX_POINT ( 'NONE', #12509 ) ;
#5101 = DIRECTION ( 'NONE',  ( 0.000000000000000000, -0.9510565162951566398, 0.3090169943749382364 ) ) ;
#5102 = ORIENTED_EDGE ( 'NONE', *, *, #6305, .F. ) ;
#5103 = ORIENTED_EDGE ( 'NONE', *, *, #6598, .F. ) ;
#5104 = APPLICATION_PROTOCOL_DEFINITION ( 'draft international standard', 'automotive_design', 1998, #17729 ) ;
#5105 = AXIS2_PLACEMENT_3D ( 'NONE', #16731, #20494, #5251 ) ;
#5106 = DIRECTION ( 'NONE',  ( 0.000000000000000000, 0.2756373558169932236, 0.9612616959383206705 ) ) ;
#5107 = ORIENTED_EDGE ( 'NONE', *, *, #6656, .F. ) ;
#5108 = AXIS2_PLACEMENT_3D ( 'NONE', #7992, #14722, #9736 ) ;
#5109 = DIRECTION ( 'NONE',  ( -1.000000000000000000, -0.000000000000000000, -0.000000000000000000 ) ) ;
#5110 = CARTESIAN_POINT ( 'NONE',  ( 10.00000000000000000, 0.000000000000000000, 0.000000000000000000 ) ) ;
#5111 = CARTESIAN_POINT ( 'NONE',  ( 10.00000000000000000, -85.05652083079337444, 0.7600687895857258791 ) ) ;
#5112 = ADVANCED_FACE ( 'NONE', ( #10340 ), #13667, .T. ) ;
#5113 = CARTESIAN_POINT ( 'NONE',  ( 10.00000000000000000, -27.26034713664092379, -7.182859710736426706 ) ) ;
#5114 = FACE_OUTER_BOUND ( 'NONE', #4060, .T. ) ;
#5115 = DIRECTION ( 'NONE',  ( -1.000000000000000000, -0.000000000000000000, -0.000000000000000000 ) ) ;
#5116 = DIRECTION ( 'NONE',  ( 1.000000000000000000, 0.000000000000000000, 0.000000000000000000 ) ) ;
#5117 = CIRCLE ( 'NONE', #12494, 92.50100000000000477 ) ;
#5118 = AXIS2_PLACEMENT_3D ( 'NONE', #13347, #8273, #16666 ) ;
#5119 = ORIENTED_EDGE ( 'NONE', *, *, #11721, .F. ) ;
#5120 = EDGE_CURVE ( 'NONE', #7280, #13685, #4935, .T. ) ;
#5121 = VECTOR ( 'NONE', #11693, 1000.000000000000000 ) ;
#5122 = CIRCLE ( 'NONE', #6879, 32.00000000000000000 ) ;
#5123 = AXIS2_PLACEMENT_3D ( 'NONE', #5956, #21196, #4182 ) ;
#5124 = CYLINDRICAL_SURFACE ( 'NONE', #6660, 11.99999999999999645 ) ;
#5125 = EDGE_CURVE ( 'NONE', #8987, #6547, #195, .T. ) ;
#5126 = DIRECTION ( 'NONE',  ( -1.000000000000000000, -0.000000000000000000, 0.000000000000000000 ) ) ;
#5127 = EDGE_LOOP ( 'NONE', ( #10112, #15985, #21112, #14527 ) ) ;
#5128 = CYLINDRICAL_SURFACE ( 'NONE', #18904, 44.99999999999999289 ) ;
#5129 = EDGE_LOOP ( 'NONE', ( #10770, #14684, #17287, #14844 ) ) ;
#5130 = VERTEX_POINT ( 'NONE', #799 ) ;
#5131 = DIRECTION ( 'NONE',  ( -1.000000000000000000, 0.000000000000000000, 0.000000000000000000 ) ) ;
#5132 = ORIENTED_EDGE ( 'NONE', *, *, #12743, .F. ) ;
#5133 = AXIS2_PLACEMENT_3D ( 'NONE', #16277, #17723, #7553 ) ;
#5134 = CIRCLE ( 'NONE', #1253, 45.00000000000000000 ) ;
#5135 = ORIENTED_EDGE ( 'NONE', *, *, #8124, .F. ) ;
#5136 = CARTESIAN_POINT ( 'NONE',  ( 0.000000000000000000, -31.75612719289743779, 3.943144139962448058 ) ) ;
#5137 = CARTESIAN_POINT ( 'NONE',  ( 10.00000000000000000, -19.83954325428713972, 82.71385593638686373 ) ) ;
#5138 = CIRCLE ( 'NONE', #19246, 44.99999999999999289 ) ;
#5139 = ORIENTED_EDGE ( 'NONE', *, *, #808, .T. ) ;
#5140 = AXIS2_PLACEMENT_3D ( 'NONE', #19403, #5823, #4158 ) ;
#5141 = TOROIDAL_SURFACE ( 'NONE', #17495, 5.633200000000004870, 0.02569999999999482421 ) ;
#5142 = EDGE_CURVE ( 'NONE', #6401, #845, #11792, .T. ) ;
#5143 = CARTESIAN_POINT ( 'NONE',  ( 10.00000000000000000, 90.63195040374210976, -18.50093422002330712 ) ) ;
#5144 = CARTESIAN_POINT ( 'NONE',  ( 10.00000000000000000, 25.56104204395415991, -81.12843256239638379 ) ) ;
#5145 = ADVANCED_FACE ( 'NONE', ( #7545 ), #14277, .F. ) ;
#5146 = DIRECTION ( 'NONE',  ( 0.000000000000000000, 0.8987940462991651502, 0.4383711467890813451 ) ) ;
#5147 = EDGE_CURVE ( 'NONE', #15286, #5049, #4211, .T. ) ;
#5148 = DIRECTION ( 'NONE',  ( -1.000000000000000000, 0.000000000000000000, 0.000000000000000000 ) ) ;
#5149 = CARTESIAN_POINT ( 'NONE',  ( -8.900000000000012790, 0.000000000000000000, -101.1000000000000369 ) ) ;
#5150 = CYLINDRICAL_SURFACE ( 'NONE', #5335, 44.99999999999998579 ) ;
#5151 = ADVANCED_FACE ( 'NONE', ( #1739 ), #2469, .F. ) ;
#5152 = VERTEX_POINT ( 'NONE', #16985 ) ;
#5153 = DIRECTION ( 'NONE',  ( 1.000000000000000000, 0.000000000000000000, 0.000000000000000000 ) ) ;
#5154 = DIRECTION ( 'NONE',  ( 0.000000000000000000, 0.000000000000000000, 1.000000000000000000 ) ) ;
#5155 = VERTEX_POINT ( 'NONE', #15208 ) ;
#5156 = AXIS2_PLACEMENT_3D ( 'NONE', #11387, #16145, #21232 ) ;
#5157 = AXIS2_PLACEMENT_3D ( 'NONE', #15951, #21040, #5909 ) ;
#5158 = CARTESIAN_POINT ( 'NONE',  ( 10.00000000000000000, 0.000000000000000000, 0.000000000000000000 ) ) ;
#5159 = EDGE_CURVE ( 'NONE', #13513, #18417, #18692, .T. ) ;
#5160 = CIRCLE ( 'NONE', #7626, 44.99999999999999289 ) ;
#5161 = ORIENTED_EDGE ( 'NONE', *, *, #12886, .T. ) ;
#5162 = DIRECTION ( 'NONE',  ( 0.000000000000000000, 0.000000000000000000, 1.000000000000000000 ) ) ;
#5163 = DIRECTION ( 'NONE',  ( -1.000000000000000000, -0.000000000000000000, -0.000000000000000000 ) ) ;
#5164 = ORIENTED_EDGE ( 'NONE', *, *, #7713, .F. ) ;
#5165 = CYLINDRICAL_SURFACE ( 'NONE', #6053, 92.50100000000000477 ) ;
#5166 = EDGE_CURVE ( 'NONE', #52, #1120, #15137, .T. ) ;
#5167 = ORIENTED_EDGE ( 'NONE', *, *, #18814, .F. ) ;
#5168 = VERTEX_POINT ( 'NONE', #5378 ) ;
#5169 = ORIENTED_EDGE ( 'NONE', *, *, #20300, .F. ) ;
#5170 = DIRECTION ( 'NONE',  ( 0.000000000000000000, 0.000000000000000000, 1.000000000000000000 ) ) ;
#5171 = ORIENTED_EDGE ( 'NONE', *, *, #8361, .T. ) ;
#5172 = CYLINDRICAL_SURFACE ( 'NONE', #21508, 88.00000000000000000 ) ;
#5173 = DIRECTION ( 'NONE',  ( 0.000000000000000000, -0.9945218953682722907, -0.1045284632676635739 ) ) ;
#5174 = DIRECTION ( 'NONE',  ( 0.000000000000000000, -0.5877852522924632561, -0.8090169943749545567 ) ) ;
#5175 = AXIS2_PLACEMENT_3D ( 'NONE', #1673, #8412, #15142 ) ;
#5176 = CARTESIAN_POINT ( 'NONE',  ( 0.000000000000000000, -36.39558101400191248, 80.12091913260368869 ) ) ;
#5177 = DIRECTION ( 'NONE',  ( 0.000000000000000000, 0.5877852522924743583, -0.8090169943749465631 ) ) ;
#5178 = AXIS2_PLACEMENT_3D ( 'NONE', #17041, #6781, #8637 ) ;
#5179 = ADVANCED_FACE ( 'NONE', ( #3719 ), #5172, .F. ) ;
#5180 = DIRECTION ( 'NONE',  ( 0.000000000000000000, 0.000000000000000000, 1.000000000000000000 ) ) ;
#5181 = DIRECTION ( 'NONE',  ( 0.000000000000000000, 0.000000000000000000, -1.000000000000000000 ) ) ;
#5182 = CARTESIAN_POINT ( 'NONE',  ( 10.00000000000000000, 0.000000000000000000, 0.000000000000000000 ) ) ;
#5183 = DIRECTION ( 'NONE',  ( 0.000000000000000000, 0.000000000000000000, 1.000000000000000000 ) ) ;
#5184 = EDGE_CURVE ( 'NONE', #301, #9696, #14446, .T. ) ;
#5185 = VERTEX_POINT ( 'NONE', #15541 ) ;
#5187 = AXIS2_PLACEMENT_3D ( 'NONE', #13966, #10316, #13528 ) ;
#5186 = DIRECTION ( 'NONE',  ( -1.000000000000000000, -0.000000000000000000, 0.000000000000000000 ) ) ;
#5188 = CIRCLE ( 'NONE', #8350, 27.49900000000000588 ) ;
#5189 = ORIENTED_EDGE ( 'NONE', *, *, #17441, .T. ) ;
#5190 = DIRECTION ( 'NONE',  ( -0.000000000000000000, 0.000000000000000000, 1.000000000000000000 ) ) ;
#5191 = EDGE_CURVE ( 'NONE', #142, #20213, #10857, .T. ) ;
#5192 =( GEOMETRIC_REPRESENTATION_CONTEXT ( 3 ) GLOBAL_UNCERTAINTY_ASSIGNED_CONTEXT ( ( #7912 ) ) GLOBAL_UNIT_ASSIGNED_CONTEXT ( ( #3205, #18687, #16799 ) ) REPRESENTATION_CONTEXT ( 'NONE', 'WORKASPACE' ) );
#5193 = ORIENTED_EDGE ( 'NONE', *, *, #18415, .F. ) ;
#5194 = ORIENTED_EDGE ( 'NONE', *, *, #21182, .T. ) ;
#5195 = EDGE_CURVE ( 'NONE', #14985, #2027, #15856, .T. ) ;
#5196 = EDGE_CURVE ( 'NONE', #21331, #10498, #4568, .T. ) ;
#5197 = ORIENTED_EDGE ( 'NONE', *, *, #17037, .T. ) ;
#5198 = DIRECTION ( 'NONE',  ( 1.000000000000000000, 0.000000000000000000, 0.000000000000000000 ) ) ;
#5199 = ORIENTED_EDGE ( 'NONE', *, *, #2094, .F. ) ;
#5200 = CYLINDRICAL_SURFACE ( 'NONE', #1146, 88.00000000000000000 ) ;
#5201 = DIRECTION ( 'NONE',  ( 0.000000000000000000, 0.2079116908177597312, -0.9781476007338054668 ) ) ;
#5202 = CARTESIAN_POINT ( 'NONE',  ( 10.00000000000000000, -13.56333590714035431, 28.98337314858429892 ) ) ;
#5203 = CIRCLE ( 'NONE', #17900, 32.00000000000000000 ) ;
#5204 = CARTESIAN_POINT ( 'NONE',  ( 10.00000000000000000, 21.98203405400955290, 17.64965094506551324 ) ) ;
#5205 = CIRCLE ( 'NONE', #12241, 88.00000000000000000 ) ;
#5206 = CARTESIAN_POINT ( 'NONE',  ( 10.00000000000000000, 83.03980459022454852, 18.42770452393382641 ) ) ;
#5207 = ORIENTED_EDGE ( 'NONE', *, *, #1262, .T. ) ;
#5208 = DIRECTION ( 'NONE',  ( -1.000000000000000000, 0.000000000000000000, 0.000000000000000000 ) ) ;
#5209 = VERTEX_POINT ( 'NONE', #6351 ) ;
#5210 = ORIENTED_EDGE ( 'NONE', *, *, #4655, .T. ) ;
#5211 = AXIS2_PLACEMENT_3D ( 'NONE', #12756, #17529, #20839 ) ;
#5212 = LINE ( 'NONE', #10500, #21204 ) ;
#5213 = ORIENTED_EDGE ( 'NONE', *, *, #1886, .F. ) ;
#5214 = TOROIDAL_SURFACE ( 'NONE', #18624, 6.866799999999992465, 0.02569999999999482421 ) ;
#5215 = VECTOR ( 'NONE', #2690, 1000.000000000000000 ) ;
#5216 = CARTESIAN_POINT ( 'NONE',  ( 10.00000000000000000, 4.294029059350239486, -27.86182539015961979 ) ) ;
#5217 = ORIENTED_EDGE ( 'NONE', *, *, #2414, .T. ) ;
#5218 = VERTEX_POINT ( 'NONE', #12621 ) ;
#5219 = ITEM_DEFINED_TRANSFORMATION ( 'NONE', 'NONE', #16283,  #15567 ) ;
#5220 = DIRECTION ( 'NONE',  ( 0.000000000000000000, 0.000000000000000000, 1.000000000000000000 ) ) ;
#5221 = ORIENTED_EDGE ( 'NONE', *, *, #15955, .F. ) ;
#5222 = CARTESIAN_POINT ( 'NONE',  ( 0.000000000000000000, 86.54587337002878655, 15.93147207947034971 ) ) ;
#5223 = DIRECTION ( 'NONE',  ( -1.000000000000000000, 0.000000000000000000, 0.000000000000000000 ) ) ;
#5224 = CARTESIAN_POINT ( 'NONE',  ( 0.000000000000000000, 57.47876254627143311, 62.70072803846409215 ) ) ;
#5225 = FACE_OUTER_BOUND ( 'NONE', #13660, .T. ) ;
#5226 = DIRECTION ( 'NONE',  ( -1.000000000000000000, 0.000000000000000000, 0.000000000000000000 ) ) ;
#5227 = DIRECTION ( 'NONE',  ( 0.000000000000000000, 0.000000000000000000, 1.000000000000000000 ) ) ;
#5228 = DIRECTION ( 'NONE',  ( -1.000000000000000000, -0.000000000000000000, -0.000000000000000000 ) ) ;
#5229 = CIRCLE ( 'NONE', #6999, 27.49900000000000233 ) ;
#5230 = AXIS2_PLACEMENT_3D ( 'NONE', #14628, #3029, #4909 ) ;
#5231 = AXIS2_PLACEMENT_3D ( 'NONE', #4487, #1061, #7800 ) ;
#5232 = ORIENTED_EDGE ( 'NONE', *, *, #2761, .F. ) ;
#5233 = AXIS2_PLACEMENT_3D ( 'NONE', #1259, #9864, #9747 ) ;
#5234 = FACE_OUTER_BOUND ( 'NONE', #3197, .T. ) ;
#5235 = DIRECTION ( 'NONE',  ( -1.000000000000000000, -0.000000000000000000, 0.000000000000000000 ) ) ;
#5236 = ORIENTED_EDGE ( 'NONE', *, *, #4914, .F. ) ;
#5237 = ADVANCED_FACE ( 'NONE', ( #3012 ), #16379, .F. ) ;
#5238 = CARTESIAN_POINT ( 'NONE',  ( -1.500000000000000000, 5.000000000000004441, 4.769696007084728073 ) ) ;
#5239 = ORIENTED_EDGE ( 'NONE', *, *, #18772, .T. ) ;
#5240 =( NAMED_UNIT ( * ) SI_UNIT ( $, .STERADIAN. ) SOLID_ANGLE_UNIT ( ) );
#5241 = VECTOR ( 'NONE', #19441, 1000.000000000000000 ) ;
#5242 = ORIENTED_EDGE ( 'NONE', *, *, #9355, .T. ) ;
#5243 = CARTESIAN_POINT ( 'NONE',  ( 10.00000000000000000, -81.55207211302061410, -24.17537951050148592 ) ) ;
#5244 = VERTEX_POINT ( 'NONE', #4455 ) ;
#5245 = AXIS2_PLACEMENT_3D ( 'NONE', #14708, #21455, #6337 ) ;
#5246 = ORIENTED_EDGE ( 'NONE', *, *, #3937, .F. ) ;
#5247 = LINE ( 'NONE', #15394, #1209 ) ;
#5248 = AXIS2_PLACEMENT_3D ( 'NONE', #9845, #6558, #9949 ) ;
#5249 = DIRECTION ( 'NONE',  ( 0.000000000000000000, 0.000000000000000000, 1.000000000000000000 ) ) ;
#5250 = EDGE_CURVE ( 'NONE', #16630, #13540, #12839, .T. ) ;
#5251 = DIRECTION ( 'NONE',  ( 0.000000000000000000, 0.000000000000000000, 1.000000000000000000 ) ) ;
#5252 = FACE_OUTER_BOUND ( 'NONE', #12753, .T. ) ;
#5253 = CARTESIAN_POINT ( 'NONE',  ( 0.000000000000000000, -57.47876254627184522, 62.70072803846370135 ) ) ;
#5254 = FACE_OUTER_BOUND ( 'NONE', #15752, .T. ) ;
#5255 = DIRECTION ( 'NONE',  ( 0.000000000000000000, 0.000000000000000000, 1.000000000000000000 ) ) ;
#5256 = LINE ( 'NONE', #19157, #9472 ) ;
#5257 = CIRCLE ( 'NONE', #9830, 5.633200000000004870 ) ;
#5258 = VERTEX_POINT ( 'NONE', #11300 ) ;
#5259 = CARTESIAN_POINT ( 'NONE',  ( 10.00000000000000000, 80.18694381077148137, -28.37681241246572483 ) ) ;
#5260 = AXIS2_PLACEMENT_3D ( 'NONE', #10803, #12779, #2300 ) ;
#5261 = CARTESIAN_POINT ( 'NONE',  ( 0.000000000000000000, 0.000000000000000000, 15.00000000000000000 ) ) ;
#5262 = AXIS2_PLACEMENT_3D ( 'NONE', #6397, #3173, #21725 ) ;
#5263 = EDGE_LOOP ( 'NONE', ( #1447, #12934, #14925, #13349 ) ) ;
#5264 = AXIS2_PLACEMENT_3D ( 'NONE', #1073, #4610, #19517 ) ;
#5265 = AXIS2_PLACEMENT_3D ( 'NONE', #870, #9252, #5638 ) ;
#5266 = CARTESIAN_POINT ( 'NONE',  ( 10.00000000000000000, 0.000000000000000000, 0.000000000000000000 ) ) ;
#5267 = ORIENTED_EDGE ( 'NONE', *, *, #15673, .F. ) ;
#5268 = LINE ( 'NONE', #21834, #16571 ) ;
#5269 = EDGE_CURVE ( 'NONE', #4580, #12701, #7733, .T. ) ;
#5270 = EDGE_CURVE ( 'NONE', #8367, #3730, #17628, .T. ) ;
#5271 = CARTESIAN_POINT ( 'NONE',  ( -10.00000000000002309, 1.462840601581513364E-14, 118.9000000000000199 ) ) ;
#5272 = ORIENTED_EDGE ( 'NONE', *, *, #19818, .T. ) ;
#5273 = CARTESIAN_POINT ( 'NONE',  ( 10.00000000000000000, -48.19312842678424857, -70.09002648625245513 ) ) ;
#5274 = VERTEX_POINT ( 'NONE', #16044 ) ;
#5275 = ORIENTED_EDGE ( 'NONE', *, *, #12054, .T. ) ;
#5276 = ORIENTED_EDGE ( 'NONE', *, *, #15864, .T. ) ;
#5277 = CARTESIAN_POINT ( 'NONE',  ( 0.000000000000000000, -57.06999622551850138, 66.98518889142063415 ) ) ;
#5278 = ORIENTED_EDGE ( 'NONE', *, *, #9812, .F. ) ;
#5279 = CARTESIAN_POINT ( 'NONE',  ( -10.00000000000000000, 0.000000000000000000, 0.000000000000000000 ) ) ;
#5280 = CARTESIAN_POINT ( 'NONE',  ( 10.00000000000000000, 83.89484365856912973, 26.56417150042976161 ) ) ;
#5281 = DIRECTION ( 'NONE',  ( 0.000000000000000000, 0.000000000000000000, 1.000000000000000000 ) ) ;
#5282 = AXIS2_PLACEMENT_3D ( 'NONE', #17961, #12643, #9213 ) ;
#5283 = FACE_OUTER_BOUND ( 'NONE', #19497, .T. ) ;
#5284 = CIRCLE ( 'NONE', #1047, 5.000000000000000000 ) ;
#5285 = AXIS2_PLACEMENT_3D ( 'NONE', #10250, #18872, #20430 ) ;
#5286 = LINE ( 'NONE', #20739, #14239 ) ;
#5287 = CARTESIAN_POINT ( 'NONE',  ( 5.000000000000000000, 79.38136668499741688, 37.98155635597341728 ) ) ;
#5288 = EDGE_CURVE ( 'NONE', #20437, #17903, #7391, .T. ) ;
#5289 = LINE ( 'NONE', #1851, #17568 ) ;
#5290 = DIRECTION ( 'NONE',  ( -1.000000000000000000, 0.000000000000000000, -0.000000000000000000 ) ) ;
#5291 = ORIENTED_EDGE ( 'NONE', *, *, #3566, .F. ) ;
#5292 = ADVANCED_FACE ( 'NONE', ( #4238 ), #2900, .F. ) ;
#5293 = DIRECTION ( 'NONE',  ( 0.000000000000000000, 0.000000000000000000, 1.000000000000000000 ) ) ;
#5294 = CARTESIAN_POINT ( 'NONE',  ( 0.000000000000000000, 0.000000000000000000, 0.000000000000000000 ) ) ;
#5295 = CARTESIAN_POINT ( 'NONE',  ( 10.00000000000000000, 0.000000000000000000, 0.000000000000000000 ) ) ;
#5296 = ORIENTED_EDGE ( 'NONE', *, *, #2160, .F. ) ;
#5297 = ADVANCED_FACE ( 'NONE', ( #18049 ), #6019, .F. ) ;
#5298 = DIRECTION ( 'NONE',  ( 0.000000000000000000, 0.000000000000000000, 1.000000000000000000 ) ) ;
#5299 = ADVANCED_FACE ( 'NONE', ( #14723 ), #16271, .T. ) ;
#5300 = EDGE_LOOP ( 'NONE', ( #8478, #1385, #1863, #19510 ) ) ;
#5301 = CIRCLE ( 'NONE', #4951, 32.00000000000000000 ) ;
#5302 = CYLINDRICAL_SURFACE ( 'NONE', #5591, 44.99999999999998579 ) ;
#5303 = VECTOR ( 'NONE', #15192, 1000.000000000000000 ) ;
#5304 = EDGE_LOOP ( 'NONE', ( #902, #15309, #18992, #558 ) ) ;
#5305 = EDGE_CURVE ( 'NONE', #2378, #8708, #9497, .T. ) ;
#5306 = VERTEX_POINT ( 'NONE', #2565 ) ;
#5307 = ORIENTED_EDGE ( 'NONE', *, *, #14907, .T. ) ;
#5308 = CARTESIAN_POINT ( 'NONE',  ( 0.000000000000000000, 21.65267340503250537, 89.93106657554442052 ) ) ;
#5309 = ORIENTED_EDGE ( 'NONE', *, *, #298, .F. ) ;
#5310 = DIRECTION ( 'NONE',  ( 1.000000000000000000, 0.000000000000000000, 0.000000000000000000 ) ) ;
#5311 = ADVANCED_FACE ( 'NONE', ( #6235 ), #9297, .T. ) ;
#5312 = DIRECTION ( 'NONE',  ( -1.000000000000000000, 0.000000000000000000, 0.000000000000000000 ) ) ;
#5313 = CARTESIAN_POINT ( 'NONE',  ( 10.00000000000000000, -7.409634587002906336, -27.19958299168165183 ) ) ;
#5314 = DIRECTION ( 'NONE',  ( 0.000000000000000000, 0.000000000000000000, 1.000000000000000000 ) ) ;
#5315 = CIRCLE ( 'NONE', #12023, 11.99999999999999822 ) ;
#5316 = EDGE_CURVE ( 'NONE', #3086, #17425, #1754, .T. ) ;
#5317 = LINE ( 'NONE', #20454, #8363 ) ;
#5318 = APPLICATION_CONTEXT ( 'automotive_design' ) ;
#5319 = DIRECTION ( 'NONE',  ( 0.000000000000000000, 1.000000000000000000, -1.224646799147353207E-16 ) ) ;
#5320 = ORIENTED_EDGE ( 'NONE', *, *, #7854, .F. ) ;
#5321 = EDGE_CURVE ( 'NONE', #20994, #13440, #1043, .T. ) ;
#5322 = LINE ( 'NONE', #20773, #1635 ) ;
#5323 = EDGE_LOOP ( 'NONE', ( #327, #17530, #20505, #5797 ) ) ;
#5324 = ORIENTED_EDGE ( 'NONE', *, *, #5445, .F. ) ;
#5325 = CARTESIAN_POINT ( 'NONE',  ( 10.00000000000000000, -71.33759994381919967, -58.88447872959059026 ) ) ;
#5326 = EDGE_CURVE ( 'NONE', #7775, #1381, #4337, .T. ) ;
#5327 = ORIENTED_EDGE ( 'NONE', *, *, #14613, .F. ) ;
#5328 = CIRCLE ( 'NONE', #1441, 45.00000000000000000 ) ;
#5329 = ORIENTED_EDGE ( 'NONE', *, *, #4928, .F. ) ;
#5330 = CARTESIAN_POINT ( 'NONE',  ( 0.000000000000000000, 0.000000000000000000, 0.000000000000000000 ) ) ;
#5331 = ORIENTED_EDGE ( 'NONE', *, *, #8509, .F. ) ;
#5332 = CARTESIAN_POINT ( 'NONE',  ( 9.999999999999980460, 1.393954219129475159E-14, 113.8250000000000171 ) ) ;
#5333 = DIRECTION ( 'NONE',  ( -1.000000000000000000, 0.000000000000000000, -0.000000000000000000 ) ) ;
#5334 = DIRECTION ( 'NONE',  ( -1.000000000000000000, 0.000000000000000000, -0.000000000000000000 ) ) ;
#5335 = AXIS2_PLACEMENT_3D ( 'NONE', #8139, #21603, #3158 ) ;
#5336 = DIRECTION ( 'NONE',  ( 0.000000000000000000, -0.4067366430758070917, 0.9135454576425978690 ) ) ;
#5337 = CARTESIAN_POINT ( 'NONE',  ( 1.114299999999999846, 0.000000000000000000, -6.866799999999992465 ) ) ;
#5338 = CARTESIAN_POINT ( 'NONE',  ( 8.899999999999991473, 0.000000000000000000, -100.0000000000000284 ) ) ;
#5339 = DIRECTION ( 'NONE',  ( -1.000000000000000000, -0.000000000000000000, -0.000000000000000000 ) ) ;
#5340 = MECHANICAL_DESIGN_GEOMETRIC_PRESENTATION_REPRESENTATION (  '', ( #21560 ), #11318 ) ;
#5341 = VERTEX_POINT ( 'NONE', #1033 ) ;
#5342 = EDGE_CURVE ( 'NONE', #20840, #10449, #14612, .T. ) ;
#5343 = DIRECTION ( 'NONE',  ( 1.000000000000000000, 0.000000000000000000, 0.000000000000000000 ) ) ;
#5344 = FACE_OUTER_BOUND ( 'NONE', #14190, .T. ) ;
#5345 = ORIENTED_EDGE ( 'NONE', *, *, #15969, .T. ) ;
#5346 = DIRECTION ( 'NONE',  ( 0.000000000000000000, 0.000000000000000000, 1.000000000000000000 ) ) ;
#5347 = ORIENTED_EDGE ( 'NONE', *, *, #8361, .F. ) ;
#5348 = CARTESIAN_POINT ( 'NONE',  ( 0.000000000000000000, 0.000000000000000000, 0.000000000000000000 ) ) ;
#5349 = ORIENTED_EDGE ( 'NONE', *, *, #3102, .F. ) ;
#5350 = CARTESIAN_POINT ( 'NONE',  ( 10.00000000000000000, 21.65267340503369198, -89.93106657554412209 ) ) ;
#5351 = ORIENTED_EDGE ( 'NONE', *, *, #21212, .T. ) ;
#5352 = VERTEX_POINT ( 'NONE', #12950 ) ;
#5353 =( GEOMETRIC_REPRESENTATION_CONTEXT ( 3 ) GLOBAL_UNCERTAINTY_ASSIGNED_CONTEXT ( ( #18892 ) ) GLOBAL_UNIT_ASSIGNED_CONTEXT ( ( #14064, #12395, #20487 ) ) REPRESENTATION_CONTEXT ( 'NONE', 'WORKASPACE' ) );
#5354 = DIRECTION ( 'NONE',  ( 0.000000000000000000, 0.000000000000000000, -1.000000000000000000 ) ) ;
#5355 = DIRECTION ( 'NONE',  ( 1.000000000000000000, 0.000000000000000000, -0.000000000000000000 ) ) ;
#5356 = CARTESIAN_POINT ( 'NONE',  ( 10.00000000000000000, -14.53731623274945406, 23.34226719384900761 ) ) ;
#5357 = DIRECTION ( 'NONE',  ( -1.000000000000000000, 0.000000000000000000, 0.000000000000000000 ) ) ;
#5358 = DIRECTION ( 'NONE',  ( 1.000000000000000000, 0.000000000000000000, 0.000000000000000000 ) ) ;
#5359 = CARTESIAN_POINT ( 'NONE',  ( 0.000000000000000000, 0.000000000000000000, 0.000000000000000000 ) ) ;
#5360 = CARTESIAN_POINT ( 'NONE',  ( 5.000000000000002665, -5.479102470009884485, -87.82926298292120748 ) ) ;
#5361 = CARTESIAN_POINT ( 'NONE',  ( 10.00000000000000000, 39.87723064937233630, -83.46401306393528330 ) ) ;
#5362 = VERTEX_POINT ( 'NONE', #8104 ) ;
#5363 = DIRECTION ( 'NONE',  ( 0.000000000000000000, 0.000000000000000000, 1.000000000000000000 ) ) ;
#5364 = CARTESIAN_POINT ( 'NONE',  ( 0.000000000000000000, 36.39558101400137957, 80.12091913260394449 ) ) ;
#5365 = VERTEX_POINT ( 'NONE', #8429 ) ;
#5366 = DIRECTION ( 'NONE',  ( 0.000000000000000000, 0.000000000000000000, 1.000000000000000000 ) ) ;
#5367 = ORIENTED_EDGE ( 'NONE', *, *, #5067, .T. ) ;
#5368 = LINE ( 'NONE', #5693, #20794 ) ;
#5369 = DIRECTION ( 'NONE',  ( 0.000000000000000000, 0.000000000000000000, -1.000000000000000000 ) ) ;
#5370 = VERTEX_POINT ( 'NONE', #20363 ) ;
#5371 = DIRECTION ( 'NONE',  ( 0.000000000000000000, -1.000000000000000000, -0.000000000000000000 ) ) ;
#5372 = VERTEX_POINT ( 'NONE', #5222 ) ;
#5373 = AXIS2_PLACEMENT_3D ( 'NONE', #19782, #5986, #12705 ) ;
#5374 = VERTEX_POINT ( 'NONE', #16702 ) ;
#5375 = VERTEX_POINT ( 'NONE', #18480 ) ;
#5376 = DIRECTION ( 'NONE',  ( 0.000000000000000000, 0.000000000000000000, -1.000000000000000000 ) ) ;
#5377 = VERTEX_POINT ( 'NONE', #6677 ) ;
#5378 = CARTESIAN_POINT ( 'NONE',  ( 0.000000000000000000, -70.37753541435978377, 60.02863908169610596 ) ) ;
#5379 = CYLINDRICAL_SURFACE ( 'NONE', #8648, 44.99999999999999289 ) ;
#5380 = DIRECTION ( 'NONE',  ( 0.000000000000000000, 0.000000000000000000, 1.000000000000000000 ) ) ;
#5381 = FACE_OUTER_BOUND ( 'NONE', #11751, .T. ) ;
#5382 = CARTESIAN_POINT ( 'NONE',  ( 0.000000000000000000, -57.06999622551760609, -66.98518889142141575 ) ) ;
#5383 = CARTESIAN_POINT ( 'NONE',  ( 10.00000000000000000, 46.89573839703275127, 79.73220629831503459 ) ) ;
#5384 = CONICAL_SURFACE ( 'NONE', #21263, 103.6249999999999716, 0.5675376247847775391 ) ;
#5385 = EDGE_CURVE ( 'NONE', #4539, #13627, #15152, .T. ) ;
#5386 = DIRECTION ( 'NONE',  ( 0.000000000000000000, 0.000000000000000000, 1.000000000000000000 ) ) ;
#5387 = CARTESIAN_POINT ( 'NONE',  ( -10.00000000000000000, 0.000000000000000000, 0.000000000000000000 ) ) ;
#5388 = ORIENTED_EDGE ( 'NONE', *, *, #18097, .T. ) ;
#5389 = CARTESIAN_POINT ( 'NONE',  ( 10.00000000000000000, -37.96946988134224910, 76.11510229470846411 ) ) ;
#5390 = CIRCLE ( 'NONE', #8211, 92.50100000000000477 ) ;
#5391 = DIRECTION ( 'NONE',  ( 0.000000000000000000, 0.000000000000000000, -1.000000000000000000 ) ) ;
#5392 = EDGE_CURVE ( 'NONE', #4912, #826, #4579, .T. ) ;
#5393 = AXIS2_PLACEMENT_3D ( 'NONE', #8902, #13786, #10673 ) ;
#5394 = DIRECTION ( 'NONE',  ( 1.000000000000000000, 0.000000000000000000, 0.000000000000000000 ) ) ;
#5395 = VERTEX_POINT ( 'NONE', #13489 ) ;
#5396 = FACE_OUTER_BOUND ( 'NONE', #17597, .T. ) ;
#5397 = ORIENTED_EDGE ( 'NONE', *, *, #16048, .T. ) ;
#5398 = DIRECTION ( 'NONE',  ( -1.000000000000000000, -0.000000000000000000, 0.000000000000000000 ) ) ;
#5399 = VERTEX_POINT ( 'NONE', #1795 ) ;
#5400 = EDGE_CURVE ( 'NONE', #11838, #3976, #16932, .T. ) ;
#5401 = CIRCLE ( 'NONE', #3975, 7.500000000000020428 ) ;
#5402 = ORIENTED_EDGE ( 'NONE', *, *, #13439, .T. ) ;
#5403 = ORIENTED_EDGE ( 'NONE', *, *, #4434, .F. ) ;
#5404 = CARTESIAN_POINT ( 'NONE',  ( 10.00000000000000000, 21.31452625070926743, 82.34610137166127686 ) ) ;
#5405 = VECTOR ( 'NONE', #3098, 1000.000000000000000 ) ;
#5406 = AXIS2_PLACEMENT_3D ( 'NONE', #2745, #4400, #17774 ) ;
#5407 = CARTESIAN_POINT ( 'NONE',  ( 10.00000000000000000, 0.000000000000000000, 0.000000000000000000 ) ) ;
#5408 = DIRECTION ( 'NONE',  ( 1.000000000000000000, 0.000000000000000000, 0.000000000000000000 ) ) ;
#5409 = CARTESIAN_POINT ( 'NONE',  ( 0.000000000000000000, 0.000000000000000000, 0.000000000000000000 ) ) ;
#5410 = AXIS2_PLACEMENT_3D ( 'NONE', #11656, #8550, #18402 ) ;
#5411 = UNCERTAINTY_MEASURE_WITH_UNIT (LENGTH_MEASURE( 1.000000000000000082E-05 ), #2237, 'distance_accuracy_value', 'NONE');
#5412 = ADVANCED_FACE ( 'NONE', ( #18711 ), #10071, .T. ) ;
#5413 = CARTESIAN_POINT ( 'NONE',  ( 10.00000000000000000, 74.39348546125125949, -54.97312363261338675 ) ) ;
#5414 = ADVANCED_FACE ( 'NONE', ( #3121 ), #15257, .F. ) ;
#5415 = DIRECTION ( 'NONE',  ( -0.000000000000000000, 0.000000000000000000, -1.000000000000000000 ) ) ;
#5416 = LINE ( 'NONE', #12253, #7228 ) ;
#5417 = ADVANCED_FACE ( 'NONE', ( #3336 ), #11960, .F. ) ;
#5418 = CYLINDRICAL_SURFACE ( 'NONE', #3427, 44.99999999999999289 ) ;
#5419 = CARTESIAN_POINT ( 'NONE',  ( 0.000000000000000000, 60.65279801375343993, 63.75921967137637836 ) ) ;
#5420 = ADVANCED_FACE ( 'NONE', ( #8633 ), #16821, .T. ) ;
#5421 = STYLED_ITEM ( 'NONE', ( #9798 ), #6279 ) ;
#5422 = ORIENTED_EDGE ( 'NONE', *, *, #7905, .T. ) ;
#5423 = CARTESIAN_POINT ( 'NONE',  ( 0.000000000000000000, -92.22057093985034726, 7.197311757040199431 ) ) ;
#5424 = AXIS2_PLACEMENT_3D ( 'NONE', #1928, #8671, #15401 ) ;
#5425 = ORIENTED_EDGE ( 'NONE', *, *, #11470, .T. ) ;
#5426 = CIRCLE ( 'NONE', #15285, 45.00000000000000711 ) ;
#5427 = ORIENTED_EDGE ( 'NONE', *, *, #20008, .F. ) ;
#5428 = EDGE_CURVE ( 'NONE', #16041, #5374, #6567, .T. ) ;
#5429 = LINE ( 'NONE', #18796, #7795 ) ;
#5430 = ORIENTED_EDGE ( 'NONE', *, *, #5428, .F. ) ;
#5431 = ORIENTED_EDGE ( 'NONE', *, *, #15011, .T. ) ;
#5432 = EDGE_CURVE ( 'NONE', #15380, #2483, #11367, .T. ) ;
#5433 = DIRECTION ( 'NONE',  ( 0.000000000000000000, 0.000000000000000000, 1.000000000000000000 ) ) ;
#5434 = CIRCLE ( 'NONE', #11065, 11.99999999999999822 ) ;
#5435 = VERTEX_POINT ( 'NONE', #3560 ) ;
#5436 = DIRECTION ( 'NONE',  ( -1.000000000000000000, -0.000000000000000000, -0.000000000000000000 ) ) ;
#5437 = AXIS2_PLACEMENT_3D ( 'NONE', #21254, #11195, #6127 ) ;
#5438 = CARTESIAN_POINT ( 'NONE',  ( 10.00000000000000000, -8.925965667928249303, -92.06933331948791022 ) ) ;
#5439 = DIRECTION ( 'NONE',  ( 0.000000000000000000, -1.000000000000000000, 0.000000000000000000 ) ) ;
#5440 = DIRECTION ( 'NONE',  ( -1.000000000000000000, 0.000000000000000000, 0.000000000000000000 ) ) ;
#5441 = CIRCLE ( 'NONE', #3666, 5.453125000000000000 ) ;
#5442 = CARTESIAN_POINT ( 'NONE',  ( 10.00000000000000000, -27.26034713664101972, 7.182859710736059888 ) ) ;
#5443 = CARTESIAN_POINT ( 'NONE',  ( 10.00000000000000000, 0.000000000000000000, 0.000000000000000000 ) ) ;
#5444 = DIRECTION ( 'NONE',  ( 0.000000000000000000, 0.000000000000000000, 1.000000000000000000 ) ) ;
#5445 = EDGE_CURVE ( 'NONE', #11869, #3708, #13132, .T. ) ;
#5446 = EDGE_LOOP ( 'NONE', ( #20699, #3931, #20285, #7742 ) ) ;
#5447 = CIRCLE ( 'NONE', #6519, 88.00000000000000000 ) ;
#5448 = CARTESIAN_POINT ( 'NONE',  ( 0.000000000000000000, 0.000000000000000000, 0.000000000000000000 ) ) ;
#5449 = EDGE_CURVE ( 'NONE', #18065, #16808, #11844, .T. ) ;
#5450 = CIRCLE ( 'NONE', #17797, 44.99999999999998579 ) ;
#5451 = DIRECTION ( 'NONE',  ( 1.000000000000000000, 0.000000000000000000, 0.000000000000000000 ) ) ;
#5452 = ORIENTED_EDGE ( 'NONE', *, *, #9706, .T. ) ;
#5453 = DIRECTION ( 'NONE',  ( 1.000000000000000000, 0.000000000000000000, 0.000000000000000000 ) ) ;
#5454 = EDGE_CURVE ( 'NONE', #15310, #10766, #16601, .T. ) ;
#5455 = ORIENTED_EDGE ( 'NONE', *, *, #21029, .F. ) ;
#5456 = VECTOR ( 'NONE', #21467, 1000.000000000000000 ) ;
#5457 =( NAMED_UNIT ( * ) SI_UNIT ( $, .STERADIAN. ) SOLID_ANGLE_UNIT ( ) );
#5458 = DIRECTION ( 'NONE',  ( -1.000000000000000000, -0.000000000000000000, -0.000000000000000000 ) ) ;
#5459 = VERTEX_POINT ( 'NONE', #4893 ) ;
#5460 = ORIENTED_EDGE ( 'NONE', *, *, #13942, .T. ) ;
#5461 = EDGE_CURVE ( 'NONE', #5499, #10823, #12780, .T. ) ;
#5462 = FACE_BOUND ( 'NONE', #10495, .T. ) ;
#5463 = DIRECTION ( 'NONE',  ( 0.000000000000000000, -0.9510565162951503115, -0.3090169943749573878 ) ) ;
#5464 = EDGE_CURVE ( 'NONE', #5588, #17357, #18381, .T. ) ;
#5465 = CIRCLE ( 'NONE', #2279, 44.99999999999999289 ) ;
#5466 = DIRECTION ( 'NONE',  ( 0.000000000000000000, 0.4067366430758008744, -0.9135454576426006446 ) ) ;
#5467 = LINE ( 'NONE', #7021, #3770 ) ;
#5468 = AXIS2_PLACEMENT_3D ( 'NONE', #3298, #1202, #1431 ) ;
#5469 = DIRECTION ( 'NONE',  ( 1.000000000000000000, -0.000000000000000000, -0.000000000000000000 ) ) ;
#5470 = CARTESIAN_POINT ( 'NONE',  ( 10.00000000000000000, -41.87002153499058466, -74.04114219178087808 ) ) ;
#5471 = AXIS2_PLACEMENT_3D ( 'NONE', #11577, #18329, #11245 ) ;
#5472 = CARTESIAN_POINT ( 'NONE',  ( -90.00000000000000000, 0.000000000000000000, 0.000000000000000000 ) ) ;
#5473 = DIRECTION ( 'NONE',  ( -1.000000000000000000, 0.000000000000000000, -0.000000000000000000 ) ) ;
#5474 = VECTOR ( 'NONE', #57, 1000.000000000000000 ) ;
#5475 = EDGE_LOOP ( 'NONE', ( #9933, #9813, #20290, #13084 ) ) ;
#5476 = VECTOR ( 'NONE', #9243, 1000.000000000000000 ) ;
#5477 = CARTESIAN_POINT ( 'NONE',  ( 1.500000000000000000, 15.00000000000000000, 0.000000000000000000 ) ) ;
#5478 = ORIENTED_EDGE ( 'NONE', *, *, #19343, .T. ) ;
#5479 = CARTESIAN_POINT ( 'NONE',  ( 10.00000000000000000, 0.000000000000000000, 0.000000000000000000 ) ) ;
#5480 = ORIENTED_EDGE ( 'NONE', *, *, #17937, .T. ) ;
#5481 = FACE_OUTER_BOUND ( 'NONE', #8617, .T. ) ;
#5482 = CARTESIAN_POINT ( 'NONE',  ( 0.000000000000000000, 6.797690662956386021, -87.73705831432209834 ) ) ;
#5483 = ORIENTED_EDGE ( 'NONE', *, *, #1666, .T. ) ;
#5484 = VECTOR ( 'NONE', #19622, 1000.000000000000000 ) ;
#5485 = AXIS2_PLACEMENT_3D ( 'NONE', #135, #8532, #10292 ) ;
#5486 = ORIENTED_EDGE ( 'NONE', *, *, #13236, .F. ) ;
#5487 = ORIENTED_EDGE ( 'NONE', *, *, #5982, .F. ) ;
#5488 = ORIENTED_EDGE ( 'NONE', *, *, #5550, .T. ) ;
#5489 = DIRECTION ( 'NONE',  ( 1.000000000000000000, 0.000000000000000000, -0.000000000000000000 ) ) ;
#5490 = ORIENTED_EDGE ( 'NONE', *, *, #11255, .F. ) ;
#5491 = DIRECTION ( 'NONE',  ( -1.000000000000000000, 0.000000000000000000, -0.000000000000000000 ) ) ;
#5492 = CARTESIAN_POINT ( 'NONE',  ( 10.00000000000000000, -8.134922360105496963, -84.67002113262489615 ) ) ;
#5493 = DIRECTION ( 'NONE',  ( -1.000000000000000000, 0.000000000000000000, -0.000000000000000000 ) ) ;
#5494 = LINE ( 'NONE', #12227, #8951 ) ;
#5495 = DIRECTION ( 'NONE',  ( 0.000000000000000000, -0.2079116908177468526, -0.9781476007338083534 ) ) ;
#5496 = AXIS2_PLACEMENT_3D ( 'NONE', #9507, #19358, #17923 ) ;
#5497 = CARTESIAN_POINT ( 'NONE',  ( 10.00000000000000000, -88.70892494636754577, 26.21376805916555242 ) ) ;
#5498 = CIRCLE ( 'NONE', #18550, 11.99999999999999822 ) ;
#5499 = VERTEX_POINT ( 'NONE', #4995 ) ;
#5500 = VECTOR ( 'NONE', #13853, 1000.000000000000000 ) ;
#5501 = CARTESIAN_POINT ( 'NONE',  ( 7.500000000000000000, 9.184850993605147944E-16, 3.000000000000000000 ) ) ;
#5502 = AXIS2_PLACEMENT_3D ( 'NONE', #2224, #7525, #577 ) ;
#5503 = CARTESIAN_POINT ( 'NONE',  ( 10.00000000000000000, -41.87002153499058466, -74.04114219178087808 ) ) ;
#5504 = CARTESIAN_POINT ( 'NONE',  ( 0.000000000000000000, 0.000000000000000000, 0.000000000000000000 ) ) ;
#5505 = ORIENTED_EDGE ( 'NONE', *, *, #9202, .F. ) ;
#5506 = CARTESIAN_POINT ( 'NONE',  ( 10.00000000000000000, 9.366510754379232750, 25.85466064925429208 ) ) ;
#5507 = VERTEX_POINT ( 'NONE', #11731 ) ;
#5508 = CARTESIAN_POINT ( 'NONE',  ( -10.00000000000000000, 1.224646799147353217E-14, -100.0000000000000000 ) ) ;
#5509 = ORIENTED_EDGE ( 'NONE', *, *, #5639, .F. ) ;
#5510 = VERTEX_POINT ( 'NONE', #6778 ) ;
#5511 = ADVANCED_FACE ( 'NONE', ( #18595 ), #7202, .F. ) ;
#5512 = COLOUR_RGB ( '', 0.40784314, 0.44705882, 0.49803922) ;
#5513 = ORIENTED_EDGE ( 'NONE', *, *, #14040, .T. ) ;
#5514 = AXIS2_PLACEMENT_3D ( 'NONE', #3073, #13339, #13448 ) ;
#5515 = PLANE ( 'NONE',  #19714 ) ;
#5516 = FACE_OUTER_BOUND ( 'NONE', #13482, .T. ) ;
#5517 = DIRECTION ( 'NONE',  ( 0.000000000000000000, 0.000000000000000000, -1.000000000000000000 ) ) ;
#5518 = CARTESIAN_POINT ( 'NONE',  ( -1.114300000000000290, 0.000000000000000000, -6.866799999999992465 ) ) ;
#5519 = EDGE_CURVE ( 'NONE', #10355, #4606, #15607, .T. ) ;
#5520 = DIRECTION ( 'NONE',  ( 0.000000000000000000, 0.000000000000000000, 1.000000000000000000 ) ) ;
#5521 = DIRECTION ( 'NONE',  ( 0.000000000000000000, 0.000000000000000000, 1.000000000000000000 ) ) ;
#5522 = CARTESIAN_POINT ( 'NONE',  ( 10.00000000000000000, 24.89070495400735794, 84.40647372620510680 ) ) ;
#5523 = FACE_OUTER_BOUND ( 'NONE', #12943, .T. ) ;
#5524 = DIRECTION ( 'NONE',  ( 0.000000000000000000, 0.4067366430757948237, 0.9135454576426033091 ) ) ;
#5525 = VECTOR ( 'NONE', #13026, 1000.000000000000000 ) ;
#5526 = ORIENTED_EDGE ( 'NONE', *, *, #16538, .F. ) ;
#5527 = DIRECTION ( 'NONE',  ( -1.000000000000000000, -0.000000000000000000, -0.000000000000000000 ) ) ;
#5528 = EDGE_LOOP ( 'NONE', ( #13803, #11564, #700, #4557 ) ) ;
#5529 = ORIENTED_EDGE ( 'NONE', *, *, #3818, .T. ) ;
#5530 = VERTEX_POINT ( 'NONE', #10617 ) ;
#5531 = DIRECTION ( 'NONE',  ( 0.000000000000000000, 0.000000000000000000, 1.000000000000000000 ) ) ;
#5532 = ORIENTED_EDGE ( 'NONE', *, *, #6218, .F. ) ;
#5533 = EDGE_CURVE ( 'NONE', #17607, #4746, #7148, .T. ) ;
#5534 = EDGE_CURVE ( 'NONE', #18366, #2155, #2123, .T. ) ;
#5535 = EDGE_CURVE ( 'NONE', #13186, #10390, #1850, .T. ) ;
#5536 = ORIENTED_EDGE ( 'NONE', *, *, #7209, .F. ) ;
#5537 = CARTESIAN_POINT ( 'NONE',  ( 10.00000000000000000, -84.19736439813830486, 38.30455363800902546 ) ) ;
#5538 = VECTOR ( 'NONE', #1338, 1000.000000000000000 ) ;
#5539 = ADVANCED_FACE ( 'NONE', ( #8746 ), #3884, .T. ) ;
#5540 = ORIENTED_EDGE ( 'NONE', *, *, #6527, .F. ) ;
#5541 = VECTOR ( 'NONE', #14775, 1000.000000000000000 ) ;
#5542 = DIRECTION ( 'NONE',  ( -1.000000000000000000, 0.000000000000000000, 0.000000000000000000 ) ) ;
#5543 = VECTOR ( 'NONE', #7083, 1000.000000000000000 ) ;
#5544 = CARTESIAN_POINT ( 'NONE',  ( 10.00000000000000000, -71.72924546249979016, 45.71766382684644725 ) ) ;
#5545 = DIRECTION ( 'NONE',  ( 0.000000000000000000, 0.000000000000000000, -1.000000000000000000 ) ) ;
#5546 = DIRECTION ( 'NONE',  ( 0.000000000000000000, 0.000000000000000000, 1.000000000000000000 ) ) ;
#5547 = FACE_OUTER_BOUND ( 'NONE', #15881, .T. ) ;
#5548 = CYLINDRICAL_SURFACE ( 'NONE', #15020, 7.500000000000000000 ) ;
#5549 = CARTESIAN_POINT ( 'NONE',  ( 10.00000000000000000, 0.000000000000000000, 0.000000000000000000 ) ) ;
#5550 = EDGE_CURVE ( 'NONE', #13354, #10036, #5733, .T. ) ;
#5551 = CARTESIAN_POINT ( 'NONE',  ( 10.00000000000000000, -27.82509854686807671, -4.525913221811426190 ) ) ;
#5552 = ORIENTED_EDGE ( 'NONE', *, *, #12465, .F. ) ;
#5553 = EDGE_CURVE ( 'NONE', #19849, #9701, #15702, .T. ) ;
#5554 = CIRCLE ( 'NONE', #13324, 5.612499999999999822 ) ;
#5555 = CIRCLE ( 'NONE', #14736, 0.1000000000000002554 ) ;
#5556 = CARTESIAN_POINT ( 'NONE',  ( 6.123233995736766282E-16, 15.00000000000000000, 5.000000000000000000 ) ) ;
#5557 = VECTOR ( 'NONE', #838, 1000.000000000000000 ) ;
#5558 = CARTESIAN_POINT ( 'NONE',  ( -140.0000507999999968, 0.000000000000000000, 1.000000000000000000 ) ) ;
#5559 = ORIENTED_EDGE ( 'NONE', *, *, #15860, .F. ) ;
#5560 = EDGE_CURVE ( 'NONE', #12130, #2487, #19838, .T. ) ;
#5561 = CARTESIAN_POINT ( 'NONE',  ( 0.000000000000000000, 0.000000000000000000, 0.000000000000000000 ) ) ;
#5562 = ORIENTED_EDGE ( 'NONE', *, *, #6283, .T. ) ;
#5563 = DIRECTION ( 'NONE',  ( -1.000000000000000000, 0.000000000000000000, 0.000000000000000000 ) ) ;
#5564 = EDGE_CURVE ( 'NONE', #6428, #21294, #20895, .T. ) ;
#5565 = ORIENTED_EDGE ( 'NONE', *, *, #10122, .T. ) ;
#5566 = ORIENTED_EDGE ( 'NONE', *, *, #14870, .T. ) ;
#5567 = DIRECTION ( 'NONE',  ( 1.000000000000000000, 0.000000000000000000, 0.000000000000000000 ) ) ;
#5568 = DIRECTION ( 'NONE',  ( 0.000000000000000000, 0.000000000000000000, 1.000000000000000000 ) ) ;
#5569 = VECTOR ( 'NONE', #7469, 1000.000000000000000 ) ;
#5570 = LINE ( 'NONE', #7662, #12160 ) ;
#5571 = DIRECTION ( 'NONE',  ( -1.000000000000000000, -0.000000000000000000, -0.000000000000000000 ) ) ;
#5572 = AXIS2_PLACEMENT_3D ( 'NONE', #13947, #15498, #8759 ) ;
#5573 = DIRECTION ( 'NONE',  ( -1.000000000000000000, -0.000000000000000000, -0.000000000000000000 ) ) ;
#5574 = AXIS2_PLACEMENT_3D ( 'NONE', #834, #12653, #16080 ) ;
#5575 = DIRECTION ( 'NONE',  ( 0.000000000000000000, 0.000000000000000000, 1.000000000000000000 ) ) ;
#5576 = AXIS2_PLACEMENT_3D ( 'NONE', #7784, #15853, #713 ) ;
#5577 = DIRECTION ( 'NONE',  ( -1.000000000000000000, 0.000000000000000000, 0.000000000000000000 ) ) ;
#5578 = CYLINDRICAL_SURFACE ( 'NONE', #10987, 92.50100000000000477 ) ;
#5579 = ADVANCED_FACE ( 'NONE', ( #9065 ), #17149, .F. ) ;
#5580 = ORIENTED_EDGE ( 'NONE', *, *, #3282, .F. ) ;
#5581 = ADVANCED_FACE ( 'NONE', ( #20473 ), #4102, .F. ) ;
#5582 = CIRCLE ( 'NONE', #12988, 101.1000000000000512 ) ;
#5583 = DIRECTION ( 'NONE',  ( 0.000000000000000000, -0.7431448254773999063, 0.6691306063588517983 ) ) ;
#5584 = VERTEX_POINT ( 'NONE', #15367 ) ;
#5585 = EDGE_CURVE ( 'NONE', #2910, #13186, #11732, .T. ) ;
#5586 = ADVANCED_FACE ( 'NONE', ( #8954 ), #14043, .T. ) ;
#5587 = DIRECTION ( 'NONE',  ( 1.000000000000000000, 0.000000000000000000, 0.000000000000000000 ) ) ;
#5588 = VERTEX_POINT ( 'NONE', #17479 ) ;
#5589 = AXIS2_PLACEMENT_3D ( 'NONE', #17686, #17908, #11273 ) ;
#5590 = CARTESIAN_POINT ( 'NONE',  ( 10.00000000000000000, 0.000000000000000000, 0.000000000000000000 ) ) ;
#5591 = AXIS2_PLACEMENT_3D ( 'NONE', #18880, #20857, #1975 ) ;
#5592 = VECTOR ( 'NONE', #9083, 1000.000000000000000 ) ;
#5593 = CARTESIAN_POINT ( 'NONE',  ( 10.00000000000000000, -41.87002153499162915, 74.04114219178029543 ) ) ;
#5594 = CIRCLE ( 'NONE', #20058, 44.99999999999999289 ) ;
#5595 = VERTEX_POINT ( 'NONE', #2330 ) ;
#5596 = ORIENTED_EDGE ( 'NONE', *, *, #3911, .F. ) ;
#5597 = ADVANCED_FACE ( 'NONE', ( #18803 ), #12380, .T. ) ;
#5598 = ORIENTED_EDGE ( 'NONE', *, *, #14466, .F. ) ;
#5599 = ORIENTED_EDGE ( 'NONE', *, *, #15518, .T. ) ;
#5600 = CARTESIAN_POINT ( 'NONE',  ( 10.00000000000000000, 0.000000000000000000, 0.000000000000000000 ) ) ;
#5601 = VERTEX_POINT ( 'NONE', #5332 ) ;
#5602 = LINE ( 'NONE', #4371, #12147 ) ;
#5603 = DIRECTION ( 'NONE',  ( 0.000000000000000000, -0.4067366430758072582, 0.9135454576425977580 ) ) ;
#5604 = DIRECTION ( 'NONE',  ( 0.000000000000000000, 0.000000000000000000, -1.000000000000000000 ) ) ;
#5605 = DIRECTION ( 'NONE',  ( 0.000000000000000000, 0.000000000000000000, 1.000000000000000000 ) ) ;
#5606 = CARTESIAN_POINT ( 'NONE',  ( -10.49999999999999822, 0.000000000000000000, 3.000000000000000000 ) ) ;
#5607 = AXIS2_PLACEMENT_3D ( 'NONE', #5846, #9357, #15990 ) ;
#5608 = VECTOR ( 'NONE', #2789, 1000.000000000000000 ) ;
#5609 = CARTESIAN_POINT ( 'NONE',  ( 10.00000000000000000, 28.15804365424197186, -1.358152127006073684 ) ) ;
#5610 = CIRCLE ( 'NONE', #16904, 92.50100000000000477 ) ;
#5611 = ORIENTED_EDGE ( 'NONE', *, *, #14484, .T. ) ;
#5612 = AXIS2_PLACEMENT_3D ( 'NONE', #11827, #18691, #8514 ) ;
#5613 = CARTESIAN_POINT ( 'NONE',  ( 0.000000000000000000, 78.80192417387927151, 39.16958956249325752 ) ) ;
#5614 = FACE_OUTER_BOUND ( 'NONE', #816, .T. ) ;
#5615 = ADVANCED_FACE ( 'NONE', ( #3987 ), #10723, .F. ) ;
#5616 = CARTESIAN_POINT ( 'NONE',  ( 0.000000000000000000, -24.73395913766471921, 12.01774797440568854 ) ) ;
#5617 = VERTEX_POINT ( 'NONE', #18127 ) ;
#5618 = DIRECTION ( 'NONE',  ( -1.000000000000000000, 0.000000000000000000, 0.000000000000000000 ) ) ;
#5619 = VERTEX_POINT ( 'NONE', #7519 ) ;
#5620 = CARTESIAN_POINT ( 'NONE',  ( 10.00000000000000000, 27.82509854686811224, 4.525913221811229903 ) ) ;
#5621 = ORIENTED_EDGE ( 'NONE', *, *, #11259, .F. ) ;
#5622 = VECTOR ( 'NONE', #8159, 1000.000000000000000 ) ;
#5623 = VERTEX_POINT ( 'NONE', #21322 ) ;
#5624 = AXIS2_PLACEMENT_3D ( 'NONE', #3386, #13211, #1299 ) ;
#5625 = ORIENTED_EDGE ( 'NONE', *, *, #9566, .F. ) ;
#5626 =( GEOMETRIC_REPRESENTATION_CONTEXT ( 3 ) GLOBAL_UNCERTAINTY_ASSIGNED_CONTEXT ( ( #19835 ) ) GLOBAL_UNIT_ASSIGNED_CONTEXT ( ( #9316, #21376, #10986 ) ) REPRESENTATION_CONTEXT ( 'NONE', 'WORKASPACE' ) );
#5627 = CARTESIAN_POINT ( 'NONE',  ( 9.999999999999996447, 0.000000000000000000, -101.1000000000000512 ) ) ;
#5628 = AXIS2_PLACEMENT_3D ( 'NONE', #16333, #1200, #7943 ) ;
#5629 = EDGE_LOOP ( 'NONE', ( #430, #9582, #662, #2316 ) ) ;
#5630 = DIRECTION ( 'NONE',  ( -0.000000000000000000, 0.000000000000000000, 1.000000000000000000 ) ) ;
#5631 = DIRECTION ( 'NONE',  ( -1.000000000000000000, 0.000000000000000000, -0.000000000000000000 ) ) ;
#5632 = DIRECTION ( 'NONE',  ( 0.000000000000000000, 0.000000000000000000, 1.000000000000000000 ) ) ;
#5633 = CYLINDRICAL_SURFACE ( 'NONE', #11031, 44.99999999999998579 ) ;
#5634 = CARTESIAN_POINT ( 'NONE',  ( 0.000000000000000000, -91.49386717542229519, 13.61276130276963592 ) ) ;
#5635 = CYLINDRICAL_SURFACE ( 'NONE', #15428, 92.50100000000000477 ) ;
#5636 = DIRECTION ( 'NONE',  ( 0.000000000000000000, 0.1391731009600589986, 0.9902680687415711391 ) ) ;
#5637 = CARTESIAN_POINT ( 'NONE',  ( 10.00000000000000000, 17.70753755129066320, -21.03896658273954046 ) ) ;
#5638 = DIRECTION ( 'NONE',  ( 0.000000000000000000, 0.9510565162951521989, 0.3090169943749514481 ) ) ;
#5639 = EDGE_CURVE ( 'NONE', #19613, #454, #886, .T. ) ;
#5640 = CIRCLE ( 'NONE', #3526, 88.00000000000000000 ) ;
#5641 = ORIENTED_EDGE ( 'NONE', *, *, #18514, .T. ) ;
#5642 = CIRCLE ( 'NONE', #19405, 92.50100000000000477 ) ;
#5643 = CARTESIAN_POINT ( 'NONE',  ( 0.000000000000000000, -72.53479564998751528, -44.42851404693431761 ) ) ;
#5644 = ORIENTED_EDGE ( 'NONE', *, *, #16357, .F. ) ;
#5645 = ORIENTED_EDGE ( 'NONE', *, *, #670, .T. ) ;
#5646 = PRODUCT_DEFINITION ( 'UNKNOWN', '', #5728, #12249 ) ;
#5647 = ORIENTED_EDGE ( 'NONE', *, *, #19154, .T. ) ;
#5648 = DIRECTION ( 'NONE',  ( 0.000000000000000000, 0.000000000000000000, 1.000000000000000000 ) ) ;
#5649 = VERTEX_POINT ( 'NONE', #1107 ) ;
#5650 = ORIENTED_EDGE ( 'NONE', *, *, #13213, .T. ) ;
#5651 = DIRECTION ( 'NONE',  ( -1.000000000000000000, 0.000000000000000000, 0.000000000000000000 ) ) ;
#5652 = ORIENTED_EDGE ( 'NONE', *, *, #12825, .T. ) ;
#5653 = AXIS2_PLACEMENT_3D ( 'NONE', #15382, #259, #3790 ) ;
#5654 = DIRECTION ( 'NONE',  ( -1.000000000000000000, 0.000000000000000000, 0.000000000000000000 ) ) ;
#5655 = DIRECTION ( 'NONE',  ( -1.000000000000000000, -0.000000000000000000, 0.000000000000000000 ) ) ;
#5656 = DIRECTION ( 'NONE',  ( -1.000000000000000000, -0.000000000000000000, -0.000000000000000000 ) ) ;
#5657 = CARTESIAN_POINT ( 'NONE',  ( 10.00000000000000000, 0.000000000000000000, 0.000000000000000000 ) ) ;
#5658 = DIRECTION ( 'NONE',  ( -1.000000000000000000, -0.000000000000000000, -0.000000000000000000 ) ) ;
#5659 = DIRECTION ( 'NONE',  ( 0.000000000000000000, 0.000000000000000000, 1.000000000000000000 ) ) ;
#5660 = CARTESIAN_POINT ( 'NONE',  ( 10.00000000000000000, -87.17509410653646285, 30.93441398372555540 ) ) ;
#5661 = DIRECTION ( 'NONE',  ( -1.000000000000000000, -0.000000000000000000, -0.000000000000000000 ) ) ;
#5662 = EDGE_CURVE ( 'NONE', #1841, #16217, #3266, .T. ) ;
#5663 = ORIENTED_EDGE ( 'NONE', *, *, #20802, .F. ) ;
#5664 = CIRCLE ( 'NONE', #8149, 44.99999999999999289 ) ;
#5665 = DIRECTION ( 'NONE',  ( 0.000000000000000000, 0.000000000000000000, 1.000000000000000000 ) ) ;
#5666 = FACE_OUTER_BOUND ( 'NONE', #7711, .T. ) ;
#5667 = ORIENTED_EDGE ( 'NONE', *, *, #8275, .F. ) ;
#5668 = CARTESIAN_POINT ( 'NONE',  ( 0.000000000000000000, 0.000000000000000000, 0.000000000000000000 ) ) ;
#5669 = ORIENTED_EDGE ( 'NONE', *, *, #13896, .F. ) ;
#5670 = FILL_AREA_STYLE ('',( #10852 ) ) ;
#5671 = EDGE_CURVE ( 'NONE', #16156, #12184, #1499, .T. ) ;
#5672 = CARTESIAN_POINT ( 'NONE',  ( 10.00000000000000000, -78.01214607583776228, 33.90124636420084414 ) ) ;
#5673 = ORIENTED_EDGE ( 'NONE', *, *, #15577, .T. ) ;
#5674 = ORIENTED_EDGE ( 'NONE', *, *, #14559, .F. ) ;
#5675 = CARTESIAN_POINT ( 'NONE',  ( 5.000000000000000888, -31.88200538760792213, -2.745493118647322817 ) ) ;
#5676 = CARTESIAN_POINT ( 'NONE',  ( -10.00000000000000000, 0.000000000000000000, 0.000000000000000000 ) ) ;
#5677 = DIRECTION ( 'NONE',  ( 1.000000000000000000, -0.000000000000000000, 0.000000000000000000 ) ) ;
#5678 = DIRECTION ( 'NONE',  ( 0.000000000000000000, 0.000000000000000000, 1.000000000000000000 ) ) ;
#5679 =( GEOMETRIC_REPRESENTATION_CONTEXT ( 3 ) GLOBAL_UNCERTAINTY_ASSIGNED_CONTEXT ( ( #16530 ) ) GLOBAL_UNIT_ASSIGNED_CONTEXT ( ( #15634, #725, #4147 ) ) REPRESENTATION_CONTEXT ( 'NONE', 'WORKASPACE' ) );
#5680 = CARTESIAN_POINT ( 'NONE',  ( 10.00000000000000000, 19.83954325428658194, 82.71385593638699163 ) ) ;
#5681 = DIRECTION ( 'NONE',  ( 0.000000000000000000, -1.000000000000000000, 0.000000000000000000 ) ) ;
#5682 = CARTESIAN_POINT ( 'NONE',  ( 0.000000000000000000, 84.12297548659721258, -12.59025161327029529 ) ) ;
#5683 = ADVANCED_FACE ( 'NONE', ( #21004 ), #5384, .T. ) ;
#5684 = EDGE_CURVE ( 'NONE', #20304, #20166, #8203, .T. ) ;
#5685 = EDGE_CURVE ( 'NONE', #14063, #11424, #19448, .T. ) ;
#5686 = VERTEX_POINT ( 'NONE', #13039 ) ;
#5687 = DIRECTION ( 'NONE',  ( -1.000000000000000000, 0.000000000000000000, 0.000000000000000000 ) ) ;
#5688 = ADVANCED_FACE ( 'NONE', ( #4307 ), #14371, .T. ) ;
#5689 = ORIENTED_EDGE ( 'NONE', *, *, #12828, .T. ) ;
#5690 = DIRECTION ( 'NONE',  ( 0.000000000000000000, 0.000000000000000000, 1.000000000000000000 ) ) ;
#5691 = VERTEX_POINT ( 'NONE', #17796 ) ;
#5692 = EDGE_CURVE ( 'NONE', #1381, #16306, #12417, .T. ) ;
#5693 = CARTESIAN_POINT ( 'NONE',  ( -90.00000000000000000, 0.000000000000000000, -6.728125000000023448 ) ) ;
#5694 =( GEOMETRIC_REPRESENTATION_CONTEXT ( 3 ) GLOBAL_UNCERTAINTY_ASSIGNED_CONTEXT ( ( #13198 ) ) GLOBAL_UNIT_ASSIGNED_CONTEXT ( ( #14525, #12971, #2917 ) ) REPRESENTATION_CONTEXT ( 'NONE', 'WORKASPACE' ) );
#5695 = CARTESIAN_POINT ( 'NONE',  ( -140.0000507999999968, 0.000000000000000000, 0.000000000000000000 ) ) ;
#5696 = ORIENTED_EDGE ( 'NONE', *, *, #15173, .T. ) ;
#5697 = SHAPE_REPRESENTATION_RELATIONSHIP ( 'NONE' , 'NONE' ,  #6721, #11474 ) ;
#5698 = EDGE_CURVE ( 'NONE', #6130, #14098, #11019, .T. ) ;
#5699 = VERTEX_POINT ( 'NONE', #5989 ) ;
#5700 = ORIENTED_EDGE ( 'NONE', *, *, #8274, .T. ) ;
#5701 = EDGE_LOOP ( 'NONE', ( #17091, #1510, #14691, #9545 ) ) ;
#5702 = CARTESIAN_POINT ( 'NONE',  ( 0.000000000000000000, 90.32141448704707898, -19.96189084378133316 ) ) ;
#5703 = DIRECTION ( 'NONE',  ( -1.000000000000000000, -0.000000000000000000, 0.000000000000000000 ) ) ;
#5704 = ORIENTED_EDGE ( 'NONE', *, *, #19566, .T. ) ;
#5705 = ADVANCED_FACE ( 'NONE', ( #2653 ), #17914, .F. ) ;
#5706 = DIRECTION ( 'NONE',  ( 1.000000000000000000, -0.000000000000000000, -0.000000000000000000 ) ) ;
#5707 = CYLINDRICAL_SURFACE ( 'NONE', #14381, 32.00000000000000000 ) ;
#5708 = CARTESIAN_POINT ( 'NONE',  ( 10.00000000000000000, 88.70892494636740366, 26.21376805916615282 ) ) ;
#5709 = DIRECTION ( 'NONE',  ( 0.000000000000000000, -0.9945218953682744001, 0.1045284632676436454 ) ) ;
#5710 = EDGE_CURVE ( 'NONE', #8125, #4886, #16304, .T. ) ;
#5711 = FACE_OUTER_BOUND ( 'NONE', #20940, .T. ) ;
#5712 = CIRCLE ( 'NONE', #1830, 88.00000000000000000 ) ;
#5713 = PRESENTATION_LAYER_ASSIGNMENT (  '', '', ( #21577 ) ) ;
#5714 = ORIENTED_EDGE ( 'NONE', *, *, #12827, .T. ) ;
#5715 = LINE ( 'NONE', #629, #15156 ) ;
#5716 = EDGE_CURVE ( 'NONE', #5365, #282, #14920, .T. ) ;
#5717 = LINE ( 'NONE', #20852, #7248 ) ;
#5718 = CIRCLE ( 'NONE', #2888, 6.866799999999992465 ) ;
#5719 = CARTESIAN_POINT ( 'NONE',  ( 10.00000000000000000, 0.000000000000000000, 0.000000000000000000 ) ) ;
#5720 = ORIENTED_EDGE ( 'NONE', *, *, #21229, .T. ) ;
#5721 = PLANE ( 'NONE',  #8436 ) ;
#5722 = ORIENTED_EDGE ( 'NONE', *, *, #8001, .T. ) ;
#5723 = LINE ( 'NONE', #5508, #1362 ) ;
#5724 = VERTEX_POINT ( 'NONE', #9593 ) ;
#5725 =( REPRESENTATION_RELATIONSHIP ('NONE','NONE', #2177, #4577 ) REPRESENTATION_RELATIONSHIP_WITH_TRANSFORMATION ( #3330 )SHAPE_REPRESENTATION_RELATIONSHIP( ) );
#5726 = ORIENTED_EDGE ( 'NONE', *, *, #18676, .F. ) ;
#5727 = EDGE_LOOP ( 'NONE', ( #16650, #17474, #3625, #7744 ) ) ;
#5728 = PRODUCT_DEFINITION_FORMATION_WITH_SPECIFIED_SOURCE ( 'ANY', '', #1745, .NOT_KNOWN. ) ;
#5729 = CARTESIAN_POINT ( 'NONE',  ( 10.00000000000000000, 84.79630770241084292, -6.691460262315676033 ) ) ;
#5730 = EDGE_CURVE ( 'NONE', #3829, #1128, #5401, .T. ) ;
#5731 = EDGE_LOOP ( 'NONE', ( #10692, #17824, #13787, #20774 ) ) ;
#5732 = DIRECTION ( 'NONE',  ( 0.000000000000000000, -0.6946583704590033603, 0.7193398003386453077 ) ) ;
#5733 = CIRCLE ( 'NONE', #19491, 88.00000000000000000 ) ;
#5734 = DIRECTION ( 'NONE',  ( 0.000000000000000000, 0.000000000000000000, -1.000000000000000000 ) ) ;
#5735 = CARTESIAN_POINT ( 'NONE',  ( 5.000000000000002665, -11.59241532900569993, -87.23311244498751194 ) ) ;
#5736 = EDGE_CURVE ( 'NONE', #9520, #10561, #4682, .T. ) ;
#5737 = FILL_AREA_STYLE_COLOUR ( '', #9601 ) ;
#5738 = EDGE_CURVE ( 'NONE', #8283, #2619, #11383, .T. ) ;
#5739 = AXIS2_PLACEMENT_3D ( 'NONE', #9592, #6203, #12922 ) ;
#5740 = CYLINDRICAL_SURFACE ( 'NONE', #20913, 92.50100000000000477 ) ;
#5741 = LINE ( 'NONE', #9248, #13294 ) ;
#5742 = DIRECTION ( 'NONE',  ( -1.000000000000000000, 0.000000000000000000, 0.000000000000000000 ) ) ;
#5743 = CIRCLE ( 'NONE', #8562, 92.50100000000000477 ) ;
#5744 = CARTESIAN_POINT ( 'NONE',  ( 10.00000000000000000, 57.53593069156472239, -72.42963261300903355 ) ) ;
#5745 = CARTESIAN_POINT ( 'NONE',  ( 5.000000000000000000, 51.18896083639367589, -71.57995730992126937 ) ) ;
#5746 = ORIENTED_EDGE ( 'NONE', *, *, #4349, .F. ) ;
#5747 = FACE_OUTER_BOUND ( 'NONE', #10394, .T. ) ;
#5748 = ORIENTED_EDGE ( 'NONE', *, *, #11376, .F. ) ;
#5749 = CIRCLE ( 'NONE', #14556, 88.00000000000000000 ) ;
#5750 = ORIENTED_EDGE ( 'NONE', *, *, #6253, .T. ) ;
#5751 = ORIENTED_EDGE ( 'NONE', *, *, #20575, .F. ) ;
#5752 = VECTOR ( 'NONE', #18248, 1000.000000000000000 ) ;
#5753 = VECTOR ( 'NONE', #12247, 1000.000000000000000 ) ;
#5754 = VERTEX_POINT ( 'NONE', #16246 ) ;
#5755 = ORIENTED_EDGE ( 'NONE', *, *, #969, .F. ) ;
#5756 = AXIS2_PLACEMENT_3D ( 'NONE', #2136, #12299, #20812 ) ;
#5757 = ORIENTED_EDGE ( 'NONE', *, *, #5533, .T. ) ;
#5758 = DIRECTION ( 'NONE',  ( -1.000000000000000000, 0.000000000000000000, 0.000000000000000000 ) ) ;
#5759 = AXIS2_PLACEMENT_3D ( 'NONE', #15818, #17799, #7425 ) ;
#5760 = ORIENTED_EDGE ( 'NONE', *, *, #18758, .F. ) ;
#5761 = DIRECTION ( 'NONE',  ( -1.000000000000000000, 0.000000000000000000, 0.000000000000000000 ) ) ;
#5762 = DIRECTION ( 'NONE',  ( 1.000000000000000000, 0.000000000000000000, 0.000000000000000000 ) ) ;
#5763 = CIRCLE ( 'NONE', #4352, 45.00000000000000000 ) ;
#5764 = DIRECTION ( 'NONE',  ( 1.000000000000000000, -0.000000000000000000, -0.000000000000000000 ) ) ;
#5765 = CARTESIAN_POINT ( 'NONE',  ( -10.00000000000000000, 0.000000000000000000, 0.000000000000000000 ) ) ;
#5766 = CYLINDRICAL_SURFACE ( 'NONE', #3383, 27.49900000000000233 ) ;
#5767 = FACE_OUTER_BOUND ( 'NONE', #9508, .T. ) ;
#5768 = DIRECTION ( 'NONE',  ( -1.000000000000000000, -0.000000000000000000, -0.000000000000000000 ) ) ;
#5769 = VECTOR ( 'NONE', #18840, 1000.000000000000000 ) ;
#5770 = VECTOR ( 'NONE', #16439, 1000.000000000000000 ) ;
#5771 = VERTEX_POINT ( 'NONE', #12923 ) ;
#5772 = CIRCLE ( 'NONE', #16342, 45.00000000000000000 ) ;
#5773 = CYLINDRICAL_SURFACE ( 'NONE', #8679, 11.99999999999999822 ) ;
#5774 = CARTESIAN_POINT ( 'NONE',  ( 5.000000000000000000, -41.89587599971492438, -77.38692120905515992 ) ) ;
#5775 = FACE_OUTER_BOUND ( 'NONE', #5129, .T. ) ;
#5776 = CIRCLE ( 'NONE', #3655, 44.99999999999999289 ) ;
#5777 = VERTEX_POINT ( 'NONE', #16348 ) ;
#5778 = DIRECTION ( 'NONE',  ( 1.000000000000000000, 0.000000000000000000, 0.000000000000000000 ) ) ;
#5779 = ORIENTED_EDGE ( 'NONE', *, *, #16193, .T. ) ;
#5780 = VECTOR ( 'NONE', #8208, 1000.000000000000000 ) ;
#5781 = CYLINDRICAL_SURFACE ( 'NONE', #2573, 32.00000000000000000 ) ;
#5782 = VERTEX_POINT ( 'NONE', #1219 ) ;
#5783 = EDGE_CURVE ( 'NONE', #16840, #4926, #8075, .T. ) ;
#5784 = ORIENTED_EDGE ( 'NONE', *, *, #2437, .F. ) ;
#5785 = CARTESIAN_POINT ( 'NONE',  ( -90.00000000000000000, 0.000000000000000000, 0.000000000000000000 ) ) ;
#5786 = AXIS2_PLACEMENT_3D ( 'NONE', #16520, #4481, #17856 ) ;
#5787 = DIRECTION ( 'NONE',  ( -1.000000000000000000, -0.000000000000000000, -0.000000000000000000 ) ) ;
#5788 = DIRECTION ( 'NONE',  ( -1.000000000000000000, -0.000000000000000000, 0.000000000000000000 ) ) ;
#5789 = CARTESIAN_POINT ( 'NONE',  ( 0.000000000000000000, 0.000000000000000000, 0.000000000000000000 ) ) ;
#5790 = CARTESIAN_POINT ( 'NONE',  ( 10.00000000000000000, 41.87002153499110335, 74.04114219178059386 ) ) ;
#5791 = CARTESIAN_POINT ( 'NONE',  ( 5.000000000000002665, 24.89070495400845573, -84.40647372620476574 ) ) ;
#5792 = EDGE_CURVE ( 'NONE', #10821, #14214, #6463, .T. ) ;
#5793 = CARTESIAN_POINT ( 'NONE',  ( 10.00000000000000000, 27.40684453873988957, -16.51862198941980608 ) ) ;
#5794 = CARTESIAN_POINT ( 'NONE',  ( 10.00000000000000000, 86.66425444033963288, -32.33793443156312009 ) ) ;
#5795 = DIRECTION ( 'NONE',  ( 0.000000000000000000, 0.000000000000000000, 1.000000000000000000 ) ) ;
#5796 = CIRCLE ( 'NONE', #9321, 92.50100000000000477 ) ;
#5797 = ORIENTED_EDGE ( 'NONE', *, *, #6305, .T. ) ;
#5798 = FACE_OUTER_BOUND ( 'NONE', #1327, .T. ) ;
#5799 = AXIS2_PLACEMENT_3D ( 'NONE', #16294, #6377, #16632 ) ;
#5800 = ORIENTED_EDGE ( 'NONE', *, *, #19314, .T. ) ;
#5801 = VECTOR ( 'NONE', #20030, 1000.000000000000000 ) ;
#5802 = CARTESIAN_POINT ( 'NONE',  ( 0.000000000000000000, 25.48117629651203941, -10.33947075754235989 ) ) ;
#5803 = ORIENTED_EDGE ( 'NONE', *, *, #13234, .T. ) ;
#5804 = LINE ( 'NONE', #3819, #12318 ) ;
#5805 = FACE_OUTER_BOUND ( 'NONE', #10011, .T. ) ;
#5806 = VERTEX_POINT ( 'NONE', #10160 ) ;
#5807 =( NAMED_UNIT ( * ) PLANE_ANGLE_UNIT ( ) SI_UNIT ( $, .RADIAN. ) );
#5808 = AXIS2_PLACEMENT_3D ( 'NONE', #15677, #17130, #656 ) ;
#5809 = VERTEX_POINT ( 'NONE', #11495 ) ;
#5810 = EDGE_LOOP ( 'NONE', ( #11980, #14903, #21542, #19256 ) ) ;
#5811 = EDGE_CURVE ( 'NONE', #12482, #21814, #16796, .T. ) ;
#5813 = EDGE_CURVE ( 'NONE', #13984, #16102, #13140, .T. ) ;
#5812 = VECTOR ( 'NONE', #17400, 1000.000000000000000 ) ;
#5814 = ORIENTED_EDGE ( 'NONE', *, *, #20119, .F. ) ;
#5815 = ADVANCED_FACE ( 'NONE', ( #11935 ), #19858, .T. ) ;
#5816 = PLANE ( 'NONE',  #11777 ) ;
#5817 = DIRECTION ( 'NONE',  ( -1.000000000000000000, 0.000000000000000000, 0.000000000000000000 ) ) ;
#5818 = ORIENTED_EDGE ( 'NONE', *, *, #8163, .F. ) ;
#5819 = AXIS2_PLACEMENT_3D ( 'NONE', #270, #15184, #3255 ) ;
#5820 = EDGE_CURVE ( 'NONE', #5724, #17876, #19886, .T. ) ;
#5821 = DIRECTION ( 'NONE',  ( 0.000000000000000000, -0.6946583704589885944, -0.7193398003386594075 ) ) ;
#5822 = LINE ( 'NONE', #4041, #7002 ) ;
#5823 = DIRECTION ( 'NONE',  ( -1.000000000000000000, 0.000000000000000000, 0.000000000000000000 ) ) ;
#5824 = CARTESIAN_POINT ( 'NONE',  ( 10.00000000000000000, -83.03980459022467642, -18.42770452393328995 ) ) ;
#5825 = VECTOR ( 'NONE', #4070, 1000.000000000000114 ) ;
#5826 = CARTESIAN_POINT ( 'NONE',  ( 0.000000000000000000, 79.38136668499790005, -37.98155635597233726 ) ) ;
#5827 = ORIENTED_EDGE ( 'NONE', *, *, #18676, .T. ) ;
#5828 = DIRECTION ( 'NONE',  ( 0.000000000000000000, 0.000000000000000000, 1.000000000000000000 ) ) ;
#5829 = EDGE_CURVE ( 'NONE', #18262, #21840, #15024, .T. ) ;
#5830 = AXIS2_PLACEMENT_3D ( 'NONE', #9573, #1197, #19324 ) ;
#5831 = CARTESIAN_POINT ( 'NONE',  ( 10.00000000000000000, -3.974475837764312569, -92.41557521768193340 ) ) ;
#5832 = CIRCLE ( 'NONE', #18186, 0.02570000000000176310 ) ;
#5833 = EDGE_CURVE ( 'NONE', #10108, #13306, #6114, .T. ) ;
#5834 = CARTESIAN_POINT ( 'NONE',  ( 10.00000000000000000, 7.619321854369562885, 26.42235673590693423 ) ) ;
#5835 = AXIS2_PLACEMENT_3D ( 'NONE', #2221, #8747, #4212 ) ;
#5836 = ORIENTED_EDGE ( 'NONE', *, *, #6411, .F. ) ;
#5837 = DIRECTION ( 'NONE',  ( -1.000000000000000000, 0.000000000000000000, 0.000000000000000000 ) ) ;
#5838 = ORIENTED_EDGE ( 'NONE', *, *, #1642, .F. ) ;
#5839 = FACE_OUTER_BOUND ( 'NONE', #21460, .T. ) ;
#5840 = ORIENTED_EDGE ( 'NONE', *, *, #8557, .T. ) ;
#5841 = EDGE_LOOP ( 'NONE', ( #6043, #12072, #13711, #5139 ) ) ;
#5842 = ORIENTED_EDGE ( 'NONE', *, *, #19542, .F. ) ;
#5843 = AXIS2_PLACEMENT_3D ( 'NONE', #7903, #16521, #3251 ) ;
#5844 = DIRECTION ( 'NONE',  ( -1.000000000000000000, -0.000000000000000000, 0.000000000000000000 ) ) ;
#5845 = ORIENTED_EDGE ( 'NONE', *, *, #4058, .F. ) ;
#5846 = CARTESIAN_POINT ( 'NONE',  ( 10.00000000000000000, 72.53479564998782791, 44.42851404693380601 ) ) ;
#5847 = EDGE_CURVE ( 'NONE', #5258, #4988, #99, .T. ) ;
#5848 = DIRECTION ( 'NONE',  ( 1.000000000000000000, -0.000000000000000000, -0.000000000000000000 ) ) ;
#5849 = CARTESIAN_POINT ( 'NONE',  ( 0.000000000000000000, -67.05625154133410604, -63.71729851637880415 ) ) ;
#5850 = CIRCLE ( 'NONE', #6550, 5.612499999999999822 ) ;
#5851 = CIRCLE ( 'NONE', #14654, 11.99999999999999645 ) ;
#5852 = DIRECTION ( 'NONE',  ( 0.000000000000000000, -0.2756373558170063798, 0.9612616959383167847 ) ) ;
#5853 = AXIS2_PLACEMENT_3D ( 'NONE', #15289, #167, #3910 ) ;
#5854 = CARTESIAN_POINT ( 'NONE',  ( 10.00000000000000000, 15.25521607131237722, -23.70650506194154872 ) ) ;
#5855 = DIRECTION ( 'NONE',  ( 0.000000000000000000, 0.000000000000000000, 1.000000000000000000 ) ) ;
#5856 = DIRECTION ( 'NONE',  ( 0.000000000000000000, 0.000000000000000000, 1.000000000000000000 ) ) ;
#5857 = LINE ( 'NONE', #15902, #12608 ) ;
#5858 = DIRECTION ( 'NONE',  ( -1.000000000000000000, -0.000000000000000000, -0.000000000000000000 ) ) ;
#5859 = EDGE_CURVE ( 'NONE', #13685, #21583, #21652, .T. ) ;
#5860 = ADVANCED_FACE ( 'NONE', ( #2980 ), #8405, .F. ) ;
#5861 = CARTESIAN_POINT ( 'NONE',  ( -90.00000000000000000, 0.000000000000000000, -6.728125000000022560 ) ) ;
#5862 = ORIENTED_EDGE ( 'NONE', *, *, #3134, .T. ) ;
#5863 = AXIS2_PLACEMENT_3D ( 'NONE', #20400, #16971, #13539 ) ;
#5864 = VERTEX_POINT ( 'NONE', #6430 ) ;
#5865 = EDGE_CURVE ( 'NONE', #966, #6505, #5749, .T. ) ;
#5866 = AXIS2_PLACEMENT_3D ( 'NONE', #3918, #10872, #10647 ) ;
#5867 = CIRCLE ( 'NONE', #3053, 92.50100000000003320 ) ;
#5868 = ADVANCED_FACE ( 'NONE', ( #6536, #3096 ), #8, .F. ) ;
#5869 = ORIENTED_EDGE ( 'NONE', *, *, #11821, .F. ) ;
#5870 = CIRCLE ( 'NONE', #18223, 123.5000000000000142 ) ;
#5871 = VERTEX_POINT ( 'NONE', #13253 ) ;
#5872 = EDGE_LOOP ( 'NONE', ( #6278, #501, #11103, #9344 ) ) ;
#5873 = CARTESIAN_POINT ( 'NONE',  ( 10.00000000000000000, 32.56745702629739014, 78.57830605990665163 ) ) ;
#5874 = VERTEX_POINT ( 'NONE', #18358 ) ;
#5875 = CARTESIAN_POINT ( 'NONE',  ( 0.000000000000000000, 35.18804927320642406, -80.65854690202642985 ) ) ;
#5876 = DIRECTION ( 'NONE',  ( 0.000000000000000000, 0.000000000000000000, 1.000000000000000000 ) ) ;
#5877 = DIRECTION ( 'NONE',  ( 0.000000000000000000, 0.2079116908177532919, 0.9781476007338070211 ) ) ;
#5878 = DIRECTION ( 'NONE',  ( -1.000000000000000000, -0.000000000000000000, -0.000000000000000000 ) ) ;
#5879 = AXIS2_PLACEMENT_3D ( 'NONE', #15354, #15684, #20557 ) ;
#5880 = CARTESIAN_POINT ( 'NONE',  ( 5.000000000000000000, 19.29292659244005392, 25.53004080487768590 ) ) ;
#5881 = CIRCLE ( 'NONE', #16820, 44.99999999999999289 ) ;
#5882 = DIRECTION ( 'NONE',  ( 1.000000000000000000, 0.000000000000000000, 0.000000000000000000 ) ) ;
#5883 = LINE ( 'NONE', #10949, #19802 ) ;
#5884 = DIRECTION ( 'NONE',  ( -1.000000000000000000, 0.000000000000000000, 0.000000000000000000 ) ) ;
#5885 = ORIENTED_EDGE ( 'NONE', *, *, #18533, .F. ) ;
#5886 = CARTESIAN_POINT ( 'NONE',  ( 0.000000000000000000, 81.34229909304724515, -33.57723005635285318 ) ) ;
#5887 = CYLINDRICAL_SURFACE ( 'NONE', #9449, 92.50100000000000477 ) ;
#5888 = AXIS2_PLACEMENT_3D ( 'NONE', #18031, #2879, #9599 ) ;
#5889 = DIRECTION ( 'NONE',  ( 0.000000000000000000, 0.9702957262759954737, 0.2419218955996715048 ) ) ;
#5890 = ORIENTED_EDGE ( 'NONE', *, *, #3966, .F. ) ;
#5891 = AXIS2_PLACEMENT_3D ( 'NONE', #9481, #17572, #19433 ) ;
#5892 = CARTESIAN_POINT ( 'NONE',  ( 0.000000000000000000, 0.000000000000000000, 0.000000000000000000 ) ) ;
#5893 = VERTEX_POINT ( 'NONE', #3202 ) ;
#5894 = AXIS2_PLACEMENT_3D ( 'NONE', #11167, #14588, #13257 ) ;
#5895 = DIRECTION ( 'NONE',  ( 1.000000000000000000, 0.000000000000000000, 0.000000000000000000 ) ) ;
#5896 = ORIENTED_EDGE ( 'NONE', *, *, #21572, .T. ) ;
#5897 = VERTEX_POINT ( 'NONE', #1768 ) ;
#5898 = FACE_OUTER_BOUND ( 'NONE', #7369, .T. ) ;
#5899 = CARTESIAN_POINT ( 'NONE',  ( 10.00000000000000000, 8.134922360106093819, 84.67002113262482510 ) ) ;
#5900 = CARTESIAN_POINT ( 'NONE',  ( 10.00000000000000000, 87.17509410653623547, 30.93441398372612738 ) ) ;
#5901 = DIRECTION ( 'NONE',  ( -1.000000000000000000, -0.000000000000000000, -0.000000000000000000 ) ) ;
#5902 = CARTESIAN_POINT ( 'NONE',  ( 0.000000000000000000, 87.17509410653623547, 30.93441398372613094 ) ) ;
#5903 = CYLINDRICAL_SURFACE ( 'NONE', #19193, 44.99999999999998579 ) ;
#5904 = CARTESIAN_POINT ( 'NONE',  ( 5.000000000000000000, -72.58367602204218372, 49.75550195834843237 ) ) ;
#5905 = FACE_OUTER_BOUND ( 'NONE', #19801, .T. ) ;
#5906 = CARTESIAN_POINT ( 'NONE',  ( 0.000000000000000000, -78.04699792498111321, -49.64978465107371619 ) ) ;
#5907 = EDGE_LOOP ( 'NONE', ( #13629, #3548, #14885, #3718 ) ) ;
#5908 = AXIS2_PLACEMENT_3D ( 'NONE', #18224, #13120, #6072 ) ;
#5909 = DIRECTION ( 'NONE',  ( 0.000000000000000000, -0.8660254037844431485, 0.4999999999999919509 ) ) ;
#5910 = EDGE_CURVE ( 'NONE', #3795, #20360, #2220, .T. ) ;
#5911 = EDGE_LOOP ( 'NONE', ( #12533, #7597 ) ) ;
#5912 = CARTESIAN_POINT ( 'NONE',  ( 10.00000000000000000, 29.29369617358468858, 87.74003855418408193 ) ) ;
#5913 = EDGE_LOOP ( 'NONE', ( #12862, #1563, #21194, #746 ) ) ;
#5914 = CARTESIAN_POINT ( 'NONE',  ( 7.599999999999998757, 1.287093988729475069E-14, 105.0992000000000104 ) ) ;
#5915 = ORIENTED_EDGE ( 'NONE', *, *, #13788, .F. ) ;
#5916 = PRODUCT_DEFINITION ( 'UNKNOWN', '', #16301, #20652 ) ;
#5917 = SHAPE_REPRESENTATION_RELATIONSHIP ( 'NONE' , 'NONE' ,  #21798, #14875 ) ;
#5918 = AXIS2_PLACEMENT_3D ( 'NONE', #9004, #17972, #19399 ) ;
#5919 = ORIENTED_EDGE ( 'NONE', *, *, #6598, .T. ) ;
#5920 = ORIENTED_EDGE ( 'NONE', *, *, #9361, .T. ) ;
#5921 = CIRCLE ( 'NONE', #15444, 44.99999999999999289 ) ;
#5922 = ORIENTED_EDGE ( 'NONE', *, *, #785, .T. ) ;
#5923 = FACE_OUTER_BOUND ( 'NONE', #13802, .T. ) ;
#5924 = CARTESIAN_POINT ( 'NONE',  ( 0.000000000000000000, -36.39558101400082535, -80.12091913260421450 ) ) ;
#5925 = CIRCLE ( 'NONE', #1683, 92.50100000000000477 ) ;
#5926 = VERTEX_POINT ( 'NONE', #13467 ) ;
#5927 = DIRECTION ( 'NONE',  ( 0.000000000000000000, 0.000000000000000000, 1.000000000000000000 ) ) ;
#5928 = CARTESIAN_POINT ( 'NONE',  ( 0.000000000000000000, 78.83848282823974785, -48.38314403117421847 ) ) ;
#5929 = FACE_OUTER_BOUND ( 'NONE', #12501, .T. ) ;
#5930 = CARTESIAN_POINT ( 'NONE',  ( 0.000000000000000000, -90.63195040374199607, 18.50093422002390398 ) ) ;
#5931 = AXIS2_PLACEMENT_3D ( 'NONE', #20889, #12710, #4309 ) ;
#5932 = LINE ( 'NONE', #14537, #20156 ) ;
#5933 = ORIENTED_EDGE ( 'NONE', *, *, #10816, .T. ) ;
#5934 = DIRECTION ( 'NONE',  ( 1.000000000000000000, 0.000000000000000000, 0.000000000000000000 ) ) ;
#5935 = CIRCLE ( 'NONE', #18293, 88.00000000000000000 ) ;
#5936 = CIRCLE ( 'NONE', #18638, 10.49999999999999822 ) ;
#5937 = DIRECTION ( 'NONE',  ( 0.000000000000000000, 0.000000000000000000, 1.000000000000000000 ) ) ;
#5938 = EDGE_CURVE ( 'NONE', #20049, #20543, #795, .T. ) ;
#5939 = VECTOR ( 'NONE', #20260, 1000.000000000000000 ) ;
#5940 = EDGE_CURVE ( 'NONE', #20731, #10690, #16684, .T. ) ;
#5941 = VECTOR ( 'NONE', #947, 1000.000000000000000 ) ;
#5942 = AXIS2_PLACEMENT_3D ( 'NONE', #18057, #18166, #19922 ) ;
#5943 = DIRECTION ( 'NONE',  ( 1.000000000000000000, 0.000000000000000000, 0.000000000000000000 ) ) ;
#5944 = EDGE_LOOP ( 'NONE', ( #2383, #16208, #18677, #4531 ) ) ;
#5945 = DIRECTION ( 'NONE',  ( 0.000000000000000000, 0.000000000000000000, 1.000000000000000000 ) ) ;
#5946 = ORIENTED_EDGE ( 'NONE', *, *, #7312, .F. ) ;
#5947 = DIRECTION ( 'NONE',  ( 0.000000000000000000, 0.000000000000000000, 1.000000000000000000 ) ) ;
#5948 = VERTEX_POINT ( 'NONE', #3426 ) ;
#5949 = ORIENTED_EDGE ( 'NONE', *, *, #15940, .F. ) ;
#5950 = VERTEX_POINT ( 'NONE', #12362 ) ;
#5951 = CARTESIAN_POINT ( 'NONE',  ( 10.00000000000000000, 3.974475837764916530, 92.41557521768191918 ) ) ;
#5952 = ORIENTED_EDGE ( 'NONE', *, *, #3381, .T. ) ;
#5953 = ADVANCED_FACE ( 'NONE', ( #15568 ), #10482, .T. ) ;
#5954 = DIRECTION ( 'NONE',  ( 1.000000000000000000, 0.000000000000000000, 0.000000000000000000 ) ) ;
#5955 = CIRCLE ( 'NONE', #6314, 32.00000000000000000 ) ;
#5956 = CARTESIAN_POINT ( 'NONE',  ( 0.000000000000000000, 0.000000000000000000, 0.000000000000000000 ) ) ;
#5957 = CARTESIAN_POINT ( 'NONE',  ( 10.00000000000000000, 0.000000000000000000, 88.00000000000000000 ) ) ;
#5958 = VECTOR ( 'NONE', #17659, 1000.000000000000000 ) ;
#5959 = VECTOR ( 'NONE', #11292, 1000.000000000000000 ) ;
#5960 = AXIS2_PLACEMENT_3D ( 'NONE', #17696, #5661, #19243 ) ;
#5961 = EDGE_CURVE ( 'NONE', #9187, #15746, #13491, .T. ) ;
#5962 = DIRECTION ( 'NONE',  ( -1.000000000000000000, -0.000000000000000000, -0.000000000000000000 ) ) ;
#5963 = DIRECTION ( 'NONE',  ( 1.000000000000000000, 0.000000000000000000, 0.000000000000000000 ) ) ;
#5964 = DIRECTION ( 'NONE',  ( 1.000000000000000000, 0.000000000000000000, 0.000000000000000000 ) ) ;
#5965 = CARTESIAN_POINT ( 'NONE',  ( 150.0000507999999968, 0.000000000000000000, 0.000000000000000000 ) ) ;
#5966 = DIRECTION ( 'NONE',  ( 0.000000000000000000, 0.000000000000000000, 1.000000000000000000 ) ) ;
#5967 = EDGE_CURVE ( 'NONE', #19371, #17637, #17383, .T. ) ;
#5968 = ADVANCED_FACE ( 'NONE', ( #8833 ), #18780, .F. ) ;
#5969 = EDGE_CURVE ( 'NONE', #5459, #13007, #12092, .T. ) ;
#5970 = VECTOR ( 'NONE', #6156, 1000.000000000000000 ) ;
#5971 = CARTESIAN_POINT ( 'NONE',  ( 10.00000000000000000, 0.000000000000000000, 0.000000000000000000 ) ) ;
#5972 = AXIS2_PLACEMENT_3D ( 'NONE', #19648, #4514, #7933 ) ;
#5973 = ORIENTED_EDGE ( 'NONE', *, *, #687, .T. ) ;
#5974 = ADVANCED_FACE ( 'NONE', ( #12140 ), #2305, .T. ) ;
#5975 = AXIS2_PLACEMENT_3D ( 'NONE', #6059, #6168, #6286 ) ;
#5976 = ORIENTED_EDGE ( 'NONE', *, *, #4878, .F. ) ;
#5977 = CIRCLE ( 'NONE', #8790, 3.000000000000000444 ) ;
#5978 = AXIS2_PLACEMENT_3D ( 'NONE', #18789, #13814, #3318 ) ;
#5979 = ORIENTED_EDGE ( 'NONE', *, *, #8390, .F. ) ;
#5980 = EDGE_LOOP ( 'NONE', ( #20337, #14267, #5645, #19824 ) ) ;
#5981 = ORIENTED_EDGE ( 'NONE', *, *, #18430, .T. ) ;
#5982 = EDGE_CURVE ( 'NONE', #1182, #20772, #9255, .T. ) ;
#5983 = AXIS2_PLACEMENT_3D ( 'NONE', #18923, #5115, #16946 ) ;
#5984 = LINE ( 'NONE', #16242, #5241 ) ;
#5985 = ORIENTED_EDGE ( 'NONE', *, *, #9312, .T. ) ;
#5986 = DIRECTION ( 'NONE',  ( -1.000000000000000000, -0.000000000000000000, -0.000000000000000000 ) ) ;
#5987 = EDGE_CURVE ( 'NONE', #8524, #21192, #8726, .T. ) ;
#5988 = DIRECTION ( 'NONE',  ( 1.000000000000000000, 0.000000000000000000, 0.000000000000000000 ) ) ;
#5989 = CARTESIAN_POINT ( 'NONE',  ( 0.000000000000000000, 24.73395913766479737, -12.01774797440552689 ) ) ;
#5990 = AXIS2_PLACEMENT_3D ( 'NONE', #18214, #14786, #9679 ) ;
#5991 = CARTESIAN_POINT ( 'NONE',  ( 10.00000000000000888, 4.000000000000000000, -1.000000000000000000 ) ) ;
#5992 = DIRECTION ( 'NONE',  ( -0.000000000000000000, -0.000000000000000000, -1.000000000000000000 ) ) ;
#5993 = VECTOR ( 'NONE', #8218, 1000.000000000000000 ) ;
#5994 = DIRECTION ( 'NONE',  ( 0.000000000000000000, 0.000000000000000000, 1.000000000000000000 ) ) ;
#5995 = CIRCLE ( 'NONE', #7054, 27.49900000000000233 ) ;
#5996 = VECTOR ( 'NONE', #12018, 1000.000000000000000 ) ;
#5997 = EDGE_CURVE ( 'NONE', #7490, #19853, #15622, .T. ) ;
#5998 = CARTESIAN_POINT ( 'NONE',  ( 10.00000000000000000, 0.000000000000000000, 0.000000000000000000 ) ) ;
#5999 = CARTESIAN_POINT ( 'NONE',  ( 10.00000000000000000, 65.83713140174729972, 58.39068529131218099 ) ) ;
#6000 = DIRECTION ( 'NONE',  ( -1.000000000000000000, 0.000000000000000000, 0.000000000000000000 ) ) ;
#6001 = ORIENTED_EDGE ( 'NONE', *, *, #17695, .T. ) ;
#6002 = DIRECTION ( 'NONE',  ( 1.000000000000000000, 0.000000000000000000, 0.000000000000000000 ) ) ;
#6003 = SHAPE_REPRESENTATION ( 'stationary cover', ( #15567 ), #9570 ) ;
#6004 = EDGE_CURVE ( 'NONE', #5051, #1433, #13904, .T. ) ;
#6005 = FACE_BOUND ( 'NONE', #2481, .T. ) ;
#6006 = DIRECTION ( 'NONE',  ( 1.000000000000000000, 0.000000000000000000, 0.000000000000000000 ) ) ;
#6007 = ORIENTED_EDGE ( 'NONE', *, *, #10276, .T. ) ;
#6008 = VECTOR ( 'NONE', #14948, 1000.000000000000000 ) ;
#6009 = CARTESIAN_POINT ( 'NONE',  ( 0.000000000000000000, 61.33825423015685629, 69.23910433415966281 ) ) ;
#6010 = VERTEX_POINT ( 'NONE', #6970 ) ;
#6011 = CIRCLE ( 'NONE', #18363, 45.00000000000000711 ) ;
#6012 = ORIENTED_EDGE ( 'NONE', *, *, #10919, .T. ) ;
#6013 = DIRECTION ( 'NONE',  ( 0.7218214873537089904, -4.663967640694383512E-17, 0.6920792876502513957 ) ) ;
#6014 = LINE ( 'NONE', #2797, #12120 ) ;
#6015 = ORIENTED_EDGE ( 'NONE', *, *, #10086, .F. ) ;
#6016 = VERTEX_POINT ( 'NONE', #3750 ) ;
#6017 = LINE ( 'NONE', #17715, #1225 ) ;
#6018 = ADVANCED_FACE ( 'NONE', ( #2099 ), #5633, .F. ) ;
#6019 = CYLINDRICAL_SURFACE ( 'NONE', #17994, 44.99999999999999289 ) ;
#6020 = DIRECTION ( 'NONE',  ( -1.000000000000000000, 0.000000000000000000, -0.000000000000000000 ) ) ;
#6021 = LINE ( 'NONE', #19477, #291 ) ;
#6022 = CARTESIAN_POINT ( 'NONE',  ( -10.00000000000000888, 0.000000000000000000, 0.000000000000000000 ) ) ;
#6023 = DIRECTION ( 'NONE',  ( 0.000000000000000000, 0.5877852522924740253, -0.8090169943749466741 ) ) ;
#6024 = EDGE_CURVE ( 'NONE', #20241, #6321, #6815, .T. ) ;
#6025 = DIRECTION ( 'NONE',  ( 0.000000000000000000, 0.9510565162951523099, 0.3090169943749513926 ) ) ;
#6026 = CYLINDRICAL_SURFACE ( 'NONE', #5133, 92.50100000000000477 ) ;
#6027 = FACE_OUTER_BOUND ( 'NONE', #6369, .T. ) ;
#6028 = CIRCLE ( 'NONE', #12706, 3.000000000000000000 ) ;
#6029 = ORIENTED_EDGE ( 'NONE', *, *, #18283, .F. ) ;
#6030 = DIRECTION ( 'NONE',  ( -1.000000000000000000, -0.000000000000000000, 0.000000000000000000 ) ) ;
#6031 = ORIENTED_EDGE ( 'NONE', *, *, #17033, .F. ) ;
#6032 = DIRECTION ( 'NONE',  ( 0.000000000000000000, 0.000000000000000000, 1.000000000000000000 ) ) ;
#6033 = FILL_AREA_STYLE ('',( #4473 ) ) ;
#6034 = FACE_OUTER_BOUND ( 'NONE', #4119, .T. ) ;
#6035 = VERTEX_POINT ( 'NONE', #17124 ) ;
#6036 = ORIENTED_EDGE ( 'NONE', *, *, #13525, .T. ) ;
#6037 = ORIENTED_EDGE ( 'NONE', *, *, #12107, .T. ) ;
#6038 = ORIENTED_EDGE ( 'NONE', *, *, #2972, .F. ) ;
#6039 = AXIS2_PLACEMENT_3D ( 'NONE', #18209, #19521, #16547 ) ;
#6040 = CARTESIAN_POINT ( 'NONE',  ( 0.000000000000000000, 0.000000000000000000, 0.000000000000000000 ) ) ;
#6041 = CARTESIAN_POINT ( 'NONE',  ( 0.000000000000000000, 0.000000000000000000, 0.000000000000000000 ) ) ;
#6042 = EDGE_CURVE ( 'NONE', #9782, #13000, #20212, .T. ) ;
#6043 = ORIENTED_EDGE ( 'NONE', *, *, #4332, .T. ) ;
#6044 = DIRECTION ( 'NONE',  ( 0.8432271980573223802, 6.583178742724987957E-17, 0.5375573387615476539 ) ) ;
#6045 = DIRECTION ( 'NONE',  ( 0.000000000000000000, 0.4067366430757948792, 0.9135454576426031981 ) ) ;
#6046 = FACE_OUTER_BOUND ( 'NONE', #15862, .T. ) ;
#6047 = DIRECTION ( 'NONE',  ( 1.000000000000000000, 0.000000000000000000, 0.000000000000000000 ) ) ;
#6048 = DIRECTION ( 'NONE',  ( 0.000000000000000000, -0.9271838545667908660, 0.3746065934159032440 ) ) ;
#6049 = VECTOR ( 'NONE', #18416, 1000.000000000000000 ) ;
#6050 = ORIENTED_EDGE ( 'NONE', *, *, #6078, .T. ) ;
#6051 = CARTESIAN_POINT ( 'NONE',  ( 0.000000000000000000, 0.6021240089801385142, 31.99433460282945063 ) ) ;
#6052 = DIRECTION ( 'NONE',  ( -1.000000000000000000, -0.000000000000000000, 0.000000000000000000 ) ) ;
#6053 = AXIS2_PLACEMENT_3D ( 'NONE', #187, #1837, #8577 ) ;
#6054 = MANIFOLD_SOLID_BREP ( 'Extrude-Thin2', #1264 ) ;
#6055 = DIRECTION ( 'NONE',  ( 1.000000000000000000, 0.000000000000000000, 0.000000000000000000 ) ) ;
#6056 = VERTEX_POINT ( 'NONE', #1194 ) ;
#6057 = DIRECTION ( 'NONE',  ( 1.000000000000000000, 0.000000000000000000, -0.000000000000000000 ) ) ;
#6058 = ORIENTED_EDGE ( 'NONE', *, *, #14307, .T. ) ;
#6059 = CARTESIAN_POINT ( 'NONE',  ( 0.000000000000000000, -48.19312842678519360, 70.09002648625178722 ) ) ;
#6060 = ORIENTED_EDGE ( 'NONE', *, *, #5195, .F. ) ;
#6061 = LINE ( 'NONE', #6499, #17674 ) ;
#6062 = ORIENTED_EDGE ( 'NONE', *, *, #5859, .T. ) ;
#6063 = ORIENTED_EDGE ( 'NONE', *, *, #16255, .T. ) ;
#6064 = DIRECTION ( 'NONE',  ( 0.000000000000000000, 0.000000000000000000, 1.000000000000000000 ) ) ;
#6065 = ORIENTED_EDGE ( 'NONE', *, *, #4169, .F. ) ;
#6066 = CYLINDRICAL_SURFACE ( 'NONE', #5260, 88.00000000000000000 ) ;
#6067 = LINE ( 'NONE', #19206, #5825 ) ;
#6068 = DIRECTION ( 'NONE',  ( 0.000000000000000000, 0.000000000000000000, 1.000000000000000000 ) ) ;
#6069 = EDGE_CURVE ( 'NONE', #173, #7162, #7520, .T. ) ;
#6070 = COLOUR_RGB ( '', 0.66274510, 0.83137255, 0.94901961) ;
#6071 = CYLINDRICAL_SURFACE ( 'NONE', #11769, 44.99999999999998579 ) ;
#6072 = DIRECTION ( 'NONE',  ( 0.000000000000000000, 0.000000000000000000, 1.000000000000000000 ) ) ;
#6073 = DIRECTION ( 'NONE',  ( -1.000000000000000000, -0.000000000000000000, -0.000000000000000000 ) ) ;
#6074 = ADVANCED_FACE ( 'NONE', ( #10920 ), #4075, .F. ) ;
#6075 = DIRECTION ( 'NONE',  ( 0.000000000000000000, 0.000000000000000000, -1.000000000000000000 ) ) ;
#6076 = CARTESIAN_POINT ( 'NONE',  ( 10.00000000000000000, -51.76708072107842185, -67.49339815138544907 ) ) ;
#6077 = DIRECTION ( 'NONE',  ( 1.000000000000000000, 0.000000000000000000, 0.000000000000000000 ) ) ;
#6078 = EDGE_CURVE ( 'NONE', #17973, #20213, #18820, .T. ) ;
#6079 = ORIENTED_EDGE ( 'NONE', *, *, #2488, .F. ) ;
#6080 = CARTESIAN_POINT ( 'NONE',  ( 0.000000000000000000, 7.619321854369911051, -26.42235673590683476 ) ) ;
#6081 = EDGE_LOOP ( 'NONE', ( #21046, #9106, #8844, #18266 ) ) ;
#6082 = ORIENTED_EDGE ( 'NONE', *, *, #9281, .F. ) ;
#6083 = VERTEX_POINT ( 'NONE', #4287 ) ;
#6084 = VERTEX_POINT ( 'NONE', #19318 ) ;
#6085 = DIRECTION ( 'NONE',  ( 0.000000000000000000, 2.312964634635743213E-14, -1.000000000000000000 ) ) ;
#6086 = EDGE_CURVE ( 'NONE', #1178, #6420, #12450, .T. ) ;
#6087 = VERTEX_POINT ( 'NONE', #976 ) ;
#6088 = CARTESIAN_POINT ( 'NONE',  ( 10.00000000000000000, 81.32027326007866463, 44.08455690949082850 ) ) ;
#6089 = EDGE_CURVE ( 'NONE', #13540, #9424, #14934, .T. ) ;
#6090 = EDGE_CURVE ( 'NONE', #7603, #5274, #17401, .T. ) ;
#6091 = CARTESIAN_POINT ( 'NONE',  ( 7.440711023145912151, 0.000000000000000000, 0.000000000000000000 ) ) ;
#6092 = DIRECTION ( 'NONE',  ( 1.000000000000000000, -0.000000000000000000, -0.000000000000000000 ) ) ;
#6093 = EDGE_CURVE ( 'NONE', #2453, #18773, #21089, .T. ) ;
#6094 = DIRECTION ( 'NONE',  ( -1.000000000000000000, -0.000000000000000000, -0.000000000000000000 ) ) ;
#6095 = CYLINDRICAL_SURFACE ( 'NONE', #14216, 88.00000000000000000 ) ;
#6096 = DIRECTION ( 'NONE',  ( -1.000000000000000000, 0.000000000000000000, -0.000000000000000000 ) ) ;
#6097 = DIRECTION ( 'NONE',  ( 1.000000000000000000, -0.000000000000000000, -0.000000000000000000 ) ) ;
#6098 = CARTESIAN_POINT ( 'NONE',  ( 0.000000000000000000, -69.74988376403980794, -53.65588238863407611 ) ) ;
#6099 = DIRECTION ( 'NONE',  ( 0.000000000000000000, 0.000000000000000000, 1.000000000000000000 ) ) ;
#6100 = ORIENTED_EDGE ( 'NONE', *, *, #9080, .F. ) ;
#6101 = DIRECTION ( 'NONE',  ( 1.000000000000000000, 0.000000000000000000, 0.000000000000000000 ) ) ;
#6102 = EDGE_CURVE ( 'NONE', #17425, #8447, #6832, .T. ) ;
#6103 = CIRCLE ( 'NONE', #13500, 44.99999999999998579 ) ;
#6104 = ORIENTED_EDGE ( 'NONE', *, *, #2818, .T. ) ;
#6105 = CARTESIAN_POINT ( 'NONE',  ( 10.00000000000000000, 84.80486432185190893, 36.94008646920423899 ) ) ;
#6106 = EDGE_CURVE ( 'NONE', #13328, #13109, #14458, .T. ) ;
#6107 = CYLINDRICAL_SURFACE ( 'NONE', #14117, 88.00000000000000000 ) ;
#6108 = AXIS2_PLACEMENT_3D ( 'NONE', #9171, #2655, #7751 ) ;
#6109 = EDGE_LOOP ( 'NONE', ( #15300, #9485, #16626, #17306 ) ) ;
#6110 = CARTESIAN_POINT ( 'NONE',  ( 0.000000000000000000, 0.000000000000000000, 3.000000000000000000 ) ) ;
#6111 = ORIENTED_EDGE ( 'NONE', *, *, #8779, .T. ) ;
#6112 = ORIENTED_EDGE ( 'NONE', *, *, #2440, .T. ) ;
#6113 = CARTESIAN_POINT ( 'NONE',  ( 10.00000000000000000, 14.02138820415029663, -83.89630571862271324 ) ) ;
#6114 = CIRCLE ( 'NONE', #19143, 27.49900000000000588 ) ;
#6115 = ORIENTED_EDGE ( 'NONE', *, *, #10789, .T. ) ;
#6116 = VERTEX_POINT ( 'NONE', #9571 ) ;
#6117 = CARTESIAN_POINT ( 'NONE',  ( -1.500346250137462226E-14, 60.00000000000001421, -3.000000000000000000 ) ) ;
#6118 = CARTESIAN_POINT ( 'NONE',  ( 10.00000000000000000, 0.000000000000000000, 0.000000000000000000 ) ) ;
#6119 = CIRCLE ( 'NONE', #18826, 45.00000000000000711 ) ;
#6120 = VECTOR ( 'NONE', #9359, 1000.000000000000000 ) ;
#6121 = ADVANCED_FACE ( 'NONE', ( #19651 ), #6071, .F. ) ;
#6122 = CARTESIAN_POINT ( 'NONE',  ( 10.00000000000000000, 0.000000000000000000, 0.000000000000000000 ) ) ;
#6123 = DIRECTION ( 'NONE',  ( -0.000000000000000000, -0.000000000000000000, 1.000000000000000000 ) ) ;
#6124 = CARTESIAN_POINT ( 'NONE',  ( 10.00000000000000000, 62.44821182181090791, 68.23969402963524544 ) ) ;
#6125 = CARTESIAN_POINT ( 'NONE',  ( 0.000000000000000000, 8.925965667930080727, -92.06933331948771126 ) ) ;
#6126 = AXIS2_PLACEMENT_3D ( 'NONE', #10577, #20428, #18296 ) ;
#6127 = DIRECTION ( 'NONE',  ( 0.000000000000000000, -0.9945218953682744001, 0.1045284632676437286 ) ) ;
#6128 = CARTESIAN_POINT ( 'NONE',  ( 10.00000000000000000, 0.000000000000000000, 0.000000000000000000 ) ) ;
#6129 = DIRECTION ( 'NONE',  ( -1.000000000000000000, -0.000000000000000000, 0.000000000000000000 ) ) ;
#6130 = VERTEX_POINT ( 'NONE', #16227 ) ;
#6131 = CARTESIAN_POINT ( 'NONE',  ( 10.00000000000000000, 84.19736439813806328, 38.30455363800960811 ) ) ;
#6132 = EDGE_CURVE ( 'NONE', #13321, #11004, #19531, .T. ) ;
#6133 = AXIS2_PLACEMENT_3D ( 'NONE', #17212, #1960, #5177 ) ;
#6134 = ORIENTED_EDGE ( 'NONE', *, *, #8507, .F. ) ;
#6135 = EDGE_CURVE ( 'NONE', #21594, #7164, #19874, .T. ) ;
#6136 = FACE_OUTER_BOUND ( 'NONE', #8565, .T. ) ;
#6137 = VECTOR ( 'NONE', #15519, 1000.000000000000000 ) ;
#6138 = SURFACE_STYLE_FILL_AREA ( #930 ) ;
#6139 = ADVANCED_FACE ( 'NONE', ( #7499 ), #9474, .T. ) ;
#6140 = DIRECTION ( 'NONE',  ( 0.000000000000000000, 0.000000000000000000, 1.000000000000000000 ) ) ;
#6141 = ORIENTED_EDGE ( 'NONE', *, *, #1539, .F. ) ;
#6142 = AXIS2_PLACEMENT_3D ( 'NONE', #20192, #13332, #4952 ) ;
#6143 = EDGE_CURVE ( 'NONE', #20543, #393, #10341, .T. ) ;
#6144 =( NAMED_UNIT ( * ) SI_UNIT ( $, .STERADIAN. ) SOLID_ANGLE_UNIT ( ) );
#6145 = ORIENTED_EDGE ( 'NONE', *, *, #21107, .T. ) ;
#6146 = ORIENTED_EDGE ( 'NONE', *, *, #14877, .F. ) ;
#6147 = EDGE_LOOP ( 'NONE', ( #3275, #8389 ) ) ;
#6148 = DIRECTION ( 'NONE',  ( 0.000000000000000000, -0.2079116908177666145, 0.9781476007338040235 ) ) ;
#6149 = DIRECTION ( 'NONE',  ( 1.000000000000000000, 0.000000000000000000, 0.000000000000000000 ) ) ;
#6150 = ORIENTED_EDGE ( 'NONE', *, *, #7981, .T. ) ;
#6151 = AXIS2_PLACEMENT_3D ( 'NONE', #11226, #6047, #9225 ) ;
#6152 = CARTESIAN_POINT ( 'NONE',  ( 0.000000000000000000, 25.56104204395415991, -81.12843256239638379 ) ) ;
#6153 = DIRECTION ( 'NONE',  ( 0.000000000000000000, 0.000000000000000000, -1.000000000000000000 ) ) ;
#6154 = DIRECTION ( 'NONE',  ( -1.000000000000000000, 0.000000000000000000, 0.000000000000000000 ) ) ;
#6155 = DIRECTION ( 'NONE',  ( 0.000000000000000000, 0.4067366430758011520, -0.9135454576426004225 ) ) ;
#6156 = DIRECTION ( 'NONE',  ( -0.000000000000000000, -0.000000000000000000, -1.000000000000000000 ) ) ;
#6157 =( REPRESENTATION_RELATIONSHIP ('NONE','NONE', #2177, #6003 ) REPRESENTATION_RELATIONSHIP_WITH_TRANSFORMATION ( #18377 )SHAPE_REPRESENTATION_RELATIONSHIP( ) );
#6158 = AXIS2_PLACEMENT_3D ( 'NONE', #11736, #12064, #35 ) ;
#6159 = ORIENTED_EDGE ( 'NONE', *, *, #5730, .F. ) ;
#6160 = AXIS2_PLACEMENT_3D ( 'NONE', #18068, #8017, #2922 ) ;
#6161 = DIRECTION ( 'NONE',  ( -1.000000000000000000, 0.000000000000000000, 0.000000000000000000 ) ) ;
#6162 = DIRECTION ( 'NONE',  ( 0.000000000000000000, 0.000000000000000000, 1.000000000000000000 ) ) ;
#6163 = ORIENTED_EDGE ( 'NONE', *, *, #14864, .F. ) ;
#6164 = PLANE ( 'NONE',  #14369 ) ;
#6165 = ORIENTED_EDGE ( 'NONE', *, *, #856, .T. ) ;
#6166 = CIRCLE ( 'NONE', #10734, 44.99999999999999289 ) ;
#6167 = DIRECTION ( 'NONE',  ( 0.000000000000000000, 0.000000000000000000, -1.000000000000000000 ) ) ;
#6168 = DIRECTION ( 'NONE',  ( -1.000000000000000000, -0.000000000000000000, -0.000000000000000000 ) ) ;
#6169 = ORIENTED_EDGE ( 'NONE', *, *, #21249, .F. ) ;
#6170 = CYLINDRICAL_SURFACE ( 'NONE', #8848, 123.5000000000000142 ) ;
#6171 = AXIS2_PLACEMENT_3D ( 'NONE', #10131, #17093, #13446 ) ;
#6172 = ORIENTED_EDGE ( 'NONE', *, *, #8548, .F. ) ;
#6173 = ORIENTED_EDGE ( 'NONE', *, *, #15699, .T. ) ;
#6174 = CARTESIAN_POINT ( 'NONE',  ( 1.139999999999998570, 0.000000000000000000, 0.000000000000000000 ) ) ;
#6175 = AXIS2_PLACEMENT_3D ( 'NONE', #10968, #13062, #19586 ) ;
#6176 = ORIENTED_EDGE ( 'NONE', *, *, #8082, .T. ) ;
#6177 = DIRECTION ( 'NONE',  ( 0.000000000000000000, 0.000000000000000000, 1.000000000000000000 ) ) ;
#6178 = DIRECTION ( 'NONE',  ( 0.000000000000000000, 0.000000000000000000, -1.000000000000000000 ) ) ;
#6179 = CARTESIAN_POINT ( 'NONE',  ( 8.899999999999987921, 0.000000000000000000, 0.000000000000000000 ) ) ;
#6180 = DIRECTION ( 'NONE',  ( 0.000000000000000000, 0.000000000000000000, -1.000000000000000000 ) ) ;
#6181 = AXIS2_PLACEMENT_3D ( 'NONE', #12406, #10750, #9100 ) ;
#6182 = DIRECTION ( 'NONE',  ( -1.000000000000000000, 0.000000000000000000, -0.000000000000000000 ) ) ;
#6183 = AXIS2_PLACEMENT_3D ( 'NONE', #16891, #17104, #1855 ) ;
#6184 = DIRECTION ( 'NONE',  ( 1.000000000000000000, 0.000000000000000000, 0.000000000000000000 ) ) ;
#6185 = CARTESIAN_POINT ( 'NONE',  ( 10.00000000000000000, -87.17509410653646285, 30.93441398372555540 ) ) ;
#6186 = DIRECTION ( 'NONE',  ( 1.000000000000000000, 0.000000000000000000, 0.000000000000000000 ) ) ;
#6187 = AXIS2_PLACEMENT_3D ( 'NONE', #17890, #14456, #15781 ) ;
#6188 = DIRECTION ( 'NONE',  ( -1.000000000000000000, -0.000000000000000000, 0.000000000000000000 ) ) ;
#6189 = ORIENTED_EDGE ( 'NONE', *, *, #517, .F. ) ;
#6190 = EDGE_CURVE ( 'NONE', #5588, #5691, #3301, .T. ) ;
#6191 = ORIENTED_EDGE ( 'NONE', *, *, #11673, .T. ) ;
#6192 = VERTEX_POINT ( 'NONE', #12575 ) ;
#6193 = ORIENTED_EDGE ( 'NONE', *, *, #17195, .F. ) ;
#6194 = CIRCLE ( 'NONE', #7610, 11.99999999999999822 ) ;
#6195 = VECTOR ( 'NONE', #9019, 1000.000000000000000 ) ;
#6196 = CIRCLE ( 'NONE', #6571, 44.99999999999998579 ) ;
#6197 = EDGE_CURVE ( 'NONE', #1, #11814, #863, .T. ) ;
#6198 = CIRCLE ( 'NONE', #6552, 44.99999999999999289 ) ;
#6199 = ORIENTED_EDGE ( 'NONE', *, *, #16200, .F. ) ;
#6200 = VECTOR ( 'NONE', #8204, 1000.000000000000000 ) ;
#6201 = DIRECTION ( 'NONE',  ( 0.000000000000000000, 0.000000000000000000, 1.000000000000000000 ) ) ;
#6202 = VERTEX_POINT ( 'NONE', #3403 ) ;
#6203 = DIRECTION ( 'NONE',  ( 1.000000000000000000, 0.000000000000000000, 0.000000000000000000 ) ) ;
#6204 = DIRECTION ( 'NONE',  ( 0.000000000000000000, 0.000000000000000000, -1.000000000000000000 ) ) ;
#6205 = DIRECTION ( 'NONE',  ( -1.000000000000000000, -0.000000000000000000, -0.000000000000000000 ) ) ;
#6206 = DIRECTION ( 'NONE',  ( 0.000000000000000000, 0.000000000000000000, 1.000000000000000000 ) ) ;
#6207 = DIRECTION ( 'NONE',  ( -1.000000000000000000, -0.000000000000000000, -0.000000000000000000 ) ) ;
#6208 = CIRCLE ( 'NONE', #16062, 27.49900000000000233 ) ;
#6209 = LINE ( 'NONE', #7851, #3037 ) ;
#6210 = CARTESIAN_POINT ( 'NONE',  ( 0.000000000000000000, 69.74988376404090218, -53.65588238863266213 ) ) ;
#6211 = DIRECTION ( 'NONE',  ( -1.000000000000000000, 0.000000000000000000, -0.000000000000000000 ) ) ;
#6212 = VECTOR ( 'NONE', #8301, 1000.000000000000000 ) ;
#6213 = ORIENTED_EDGE ( 'NONE', *, *, #8783, .T. ) ;
#6214 = AXIS2_PLACEMENT_3D ( 'NONE', #6602, #1724, #13317 ) ;
#6215 = CIRCLE ( 'NONE', #3021, 92.50100000000003320 ) ;
#6216 = DIRECTION ( 'NONE',  ( -1.000000000000000000, -0.000000000000000000, -0.000000000000000000 ) ) ;
#6217 = EDGE_CURVE ( 'NONE', #19144, #1974, #114, .T. ) ;
#6218 = EDGE_CURVE ( 'NONE', #13174, #6690, #2933, .T. ) ;
#6219 = EDGE_CURVE ( 'NONE', #6420, #15764, #8376, .T. ) ;
#6220 = ORIENTED_EDGE ( 'NONE', *, *, #133, .T. ) ;
#6221 = CARTESIAN_POINT ( 'NONE',  ( -140.0000507999999968, 0.000000000000000000, 0.000000000000000000 ) ) ;
#6222 = EDGE_CURVE ( 'NONE', #2259, #14712, #14585, .T. ) ;
#6223 = DIRECTION ( 'NONE',  ( 0.000000000000000000, 0.000000000000000000, 1.000000000000000000 ) ) ;
#6224 = ORIENTED_EDGE ( 'NONE', *, *, #19598, .T. ) ;
#6225 = CARTESIAN_POINT ( 'NONE',  ( -90.00000000000000000, 0.000000000000000000, 0.000000000000000000 ) ) ;
#6226 = ORIENTED_EDGE ( 'NONE', *, *, #20416, .T. ) ;
#6227 = ORIENTED_EDGE ( 'NONE', *, *, #11790, .T. ) ;
#6228 =( NAMED_UNIT ( * ) SI_UNIT ( $, .STERADIAN. ) SOLID_ANGLE_UNIT ( ) );
#6229 = DIRECTION ( 'NONE',  ( 1.000000000000000000, 0.000000000000000000, 0.000000000000000000 ) ) ;
#6230 = ORIENTED_EDGE ( 'NONE', *, *, #4300, .F. ) ;
#6231 = AXIS2_PLACEMENT_3D ( 'NONE', #13918, #350, #9050 ) ;
#6232 = ORIENTED_EDGE ( 'NONE', *, *, #1396, .T. ) ;
#6233 = CYLINDRICAL_SURFACE ( 'NONE', #7931, 44.99999999999998579 ) ;
#6234 = VECTOR ( 'NONE', #6455, 1000.000000000000000 ) ;
#6235 = FACE_OUTER_BOUND ( 'NONE', #8881, .T. ) ;
#6236 = EDGE_CURVE ( 'NONE', #3708, #7417, #3988, .T. ) ;
#6237 = VECTOR ( 'NONE', #6504, 1000.000000000000000 ) ;
#6238 = FACE_OUTER_BOUND ( 'NONE', #1212, .T. ) ;
#6239 = FACE_OUTER_BOUND ( 'NONE', #9790, .T. ) ;
#6240 = FACE_OUTER_BOUND ( 'NONE', #9565, .T. ) ;
#6241 = DIRECTION ( 'NONE',  ( -1.000000000000000000, 0.000000000000000000, 0.000000000000000000 ) ) ;
#6242 = CARTESIAN_POINT ( 'NONE',  ( -1.139999999999999680, 6.866799999999992465, 0.000000000000000000 ) ) ;
#6243 = ADVANCED_FACE ( 'NONE', ( #19979 ), #13449, .F. ) ;
#6244 = CARTESIAN_POINT ( 'NONE',  ( 5.000000000000002665, 30.71797041605925216, -82.46457599186518905 ) ) ;
#6245 = DIRECTION ( 'NONE',  ( 0.000000000000000000, 0.9945218953682728458, 0.1045284632676570791 ) ) ;
#6246 = VERTEX_POINT ( 'NONE', #6297 ) ;
#6247 = DIRECTION ( 'NONE',  ( 0.000000000000000000, 0.000000000000000000, 1.000000000000000000 ) ) ;
#6248 = VERTEX_POINT ( 'NONE', #18102 ) ;
#6249 = CIRCLE ( 'NONE', #19293, 92.50099999999999056 ) ;
#6250 = EDGE_CURVE ( 'NONE', #15205, #667, #18116, .T. ) ;
#6251 = MECHANICAL_DESIGN_GEOMETRIC_PRESENTATION_REPRESENTATION (  '', ( #15762 ), #5192 ) ;
#6252 = LINE ( 'NONE', #4680, #978 ) ;
#6253 = EDGE_CURVE ( 'NONE', #3210, #20994, #1530, .T. ) ;
#6254 = CARTESIAN_POINT ( 'NONE',  ( 10.00000000000000000, 0.000000000000000000, 0.000000000000000000 ) ) ;
#6255 = CARTESIAN_POINT ( 'NONE',  ( 0.000000000000000000, -27.87320266523496315, -88.20158487341788600 ) ) ;
#6256 = ORIENTED_EDGE ( 'NONE', *, *, #21132, .F. ) ;
#6257 = EDGE_LOOP ( 'NONE', ( #7313, #3031 ) ) ;
#6258 = VERTEX_POINT ( 'NONE', #18338 ) ;
#6259 = ORIENTED_EDGE ( 'NONE', *, *, #15928, .F. ) ;
#6260 = DIRECTION ( 'NONE',  ( 0.000000000000000000, 0.000000000000000000, 1.000000000000000000 ) ) ;
#6261 = LINE ( 'NONE', #13189, #21372 ) ;
#6262 = VERTEX_POINT ( 'NONE', #16659 ) ;
#6263 = ADVANCED_FACE ( 'NONE', ( #16881 ), #15104, .F. ) ;
#6264 = AXIS2_PLACEMENT_3D ( 'NONE', #9388, #12713, #11051 ) ;
#6265 = CARTESIAN_POINT ( 'NONE',  ( 5.000000000000000000, 18.31866948046803145, -26.23788002993705248 ) ) ;
#6266 = DIRECTION ( 'NONE',  ( 1.000000000000000000, 0.000000000000000000, 0.000000000000000000 ) ) ;
#6267 = CIRCLE ( 'NONE', #18951, 44.99999999999999289 ) ;
#6268 = DIRECTION ( 'NONE',  ( 0.000000000000000000, 0.000000000000000000, -1.000000000000000000 ) ) ;
#6269 = EDGE_CURVE ( 'NONE', #17102, #4746, #5763, .T. ) ;
#6270 = CARTESIAN_POINT ( 'NONE',  ( 10.00000000000000000, 57.53593069156472239, -72.42963261300903355 ) ) ;
#6271 = CIRCLE ( 'NONE', #17901, 92.50100000000000477 ) ;
#6272 = CARTESIAN_POINT ( 'NONE',  ( -90.00000000000000000, 0.000000000000000000, -113.8250000000000028 ) ) ;
#6273 = EDGE_CURVE ( 'NONE', #5078, #13440, #17416, .T. ) ;
#6274 = EDGE_LOOP ( 'NONE', ( #19688, #11925, #4231, #18489 ) ) ;
#6275 = EDGE_CURVE ( 'NONE', #6639, #14519, #15640, .T. ) ;
#6276 = CARTESIAN_POINT ( 'NONE',  ( 150.0000507999999968, 4.000000000000000000, 1.000000000000000000 ) ) ;
#6277 = DIRECTION ( 'NONE',  ( 0.000000000000000000, 0.7431448254773910245, 0.6691306063588617903 ) ) ;
#6278 = ORIENTED_EDGE ( 'NONE', *, *, #20321, .T. ) ;
#6279 = MANIFOLD_SOLID_BREP ( 'TeethCuts', #1959 ) ;
#6280 = CARTESIAN_POINT ( 'NONE',  ( 10.00000000000000000, 32.56745702629844175, -78.57830605990621109 ) ) ;
#6281 = VERTEX_POINT ( 'NONE', #13878 ) ;
#6282 = AXIS2_PLACEMENT_3D ( 'NONE', #2754, #18107, #1090 ) ;
#6283 = EDGE_CURVE ( 'NONE', #14005, #7793, #14998, .T. ) ;
#6284 = DIRECTION ( 'NONE',  ( 0.000000000000000000, 0.000000000000000000, 1.000000000000000000 ) ) ;
#6285 = CIRCLE ( 'NONE', #3095, 44.99999999999999289 ) ;
#6286 = DIRECTION ( 'NONE',  ( 0.000000000000000000, -1.773272886554069860E-14, -1.000000000000000000 ) ) ;
#6287 = AXIS2_PLACEMENT_3D ( 'NONE', #15213, #1963, #5180 ) ;
#6288 = ORIENTED_EDGE ( 'NONE', *, *, #8827, .F. ) ;
#6289 = DIRECTION ( 'NONE',  ( -1.000000000000000000, 0.000000000000000000, 0.000000000000000000 ) ) ;
#6290 = ORIENTED_EDGE ( 'NONE', *, *, #10492, .F. ) ;
#6291 = ORIENTED_EDGE ( 'NONE', *, *, #2082, .T. ) ;
#6292 = LINE ( 'NONE', #8258, #20633 ) ;
#6293 = EDGE_LOOP ( 'NONE', ( #3950, #8067, #6702, #14539 ) ) ;
#6294 = CYLINDRICAL_SURFACE ( 'NONE', #15499, 88.00000000000000000 ) ;
#6295 = DIRECTION ( 'NONE',  ( 0.000000000000000000, 0.000000000000000000, -1.000000000000000000 ) ) ;
#6296 = CYLINDRICAL_SURFACE ( 'NONE', #74, 32.00000000000000000 ) ;
#6297 = CARTESIAN_POINT ( 'NONE',  ( 10.00000000000000000, 41.89587599971653731, -77.38692120905427885 ) ) ;
#6298 = AXIS2_PLACEMENT_3D ( 'NONE', #2326, #20470, #241 ) ;
#6299 = VECTOR ( 'NONE', #14075, 1000.000000000000000 ) ;
#6300 = CIRCLE ( 'NONE', #15460, 45.00000000000000711 ) ;
#6301 = CARTESIAN_POINT ( 'NONE',  ( 0.000000000000000000, -84.90234713953988432, 5.175025661883520200 ) ) ;
#6302 = CARTESIAN_POINT ( 'NONE',  ( 10.00000000000000000, 65.64563793391906188, -54.09103124042745492 ) ) ;
#6303 = AXIS2_PLACEMENT_3D ( 'NONE', #17533, #19505, #15875 ) ;
#6304 = AXIS2_PLACEMENT_3D ( 'NONE', #16827, #13403, #12957 ) ;
#6305 = EDGE_CURVE ( 'NONE', #16815, #14063, #12807, .T. ) ;
#6306 = DIRECTION ( 'NONE',  ( 0.000000000000000000, 0.8660254037844363761, 0.5000000000000041078 ) ) ;
#6307 = DIRECTION ( 'NONE',  ( 1.000000000000000000, 0.000000000000000000, 0.000000000000000000 ) ) ;
#6308 = DIRECTION ( 'NONE',  ( 0.000000000000000000, 0.000000000000000000, -1.000000000000000000 ) ) ;
#6309 = VECTOR ( 'NONE', #5334, 1000.000000000000000 ) ;
#6310 = CARTESIAN_POINT ( 'NONE',  ( -8.000000000000014211, 115.1000000000000227, 0.000000000000000000 ) ) ;
#6311 = ORIENTED_EDGE ( 'NONE', *, *, #5736, .T. ) ;
#6312 = ORIENTED_EDGE ( 'NONE', *, *, #4747, .F. ) ;
#6313 = ORIENTED_EDGE ( 'NONE', *, *, #5564, .F. ) ;
#6314 = AXIS2_PLACEMENT_3D ( 'NONE', #12802, #11041, #4207 ) ;
#6315 = ORIENTED_EDGE ( 'NONE', *, *, #9039, .F. ) ;
#6316 = CIRCLE ( 'NONE', #15123, 11.99999999999999822 ) ;
#6317 = AXIS2_PLACEMENT_3D ( 'NONE', #18588, #18704, #8523 ) ;
#6318 = CIRCLE ( 'NONE', #19003, 44.99999999999999289 ) ;
#6319 = ORIENTED_EDGE ( 'NONE', *, *, #862, .F. ) ;
#6320 = CARTESIAN_POINT ( 'NONE',  ( 10.00000000000000000, 29.29369617358583255, -87.74003855418371245 ) ) ;
#6321 = VERTEX_POINT ( 'NONE', #18755 ) ;
#6322 = FACE_OUTER_BOUND ( 'NONE', #7041, .T. ) ;
#6323 = DIRECTION ( 'NONE',  ( 1.000000000000000000, 0.000000000000000000, 0.000000000000000000 ) ) ;
#6324 = DIRECTION ( 'NONE',  ( 0.000000000000000000, 0.000000000000000000, 1.000000000000000000 ) ) ;
#6325 = CARTESIAN_POINT ( 'NONE',  ( 10.00000000000000000, 12.90282758292980247, 25.06465718894781247 ) ) ;
#6326 = EDGE_CURVE ( 'NONE', #9874, #3300, #9010, .T. ) ;
#6327 = CARTESIAN_POINT ( 'NONE',  ( 0.000000000000000000, 68.36541360927188293, 50.60987712331726840 ) ) ;
#6328 = CARTESIAN_POINT ( 'NONE',  ( 10.00000000000000000, -72.58367602204151581, -49.75550195834941292 ) ) ;
#6329 = CARTESIAN_POINT ( 'NONE',  ( -10.00000000000000000, 0.000000000000000000, 0.000000000000000000 ) ) ;
#6330 = CIRCLE ( 'NONE', #18678, 88.00000000000000000 ) ;
#6331 = AXIS2_PLACEMENT_3D ( 'NONE', #8039, #2841, #11451 ) ;
#6332 = VERTEX_POINT ( 'NONE', #12013 ) ;
#6333 = AXIS2_PLACEMENT_3D ( 'NONE', #6076, #20771, #4084 ) ;
#6334 = CARTESIAN_POINT ( 'NONE',  ( 10.00000000000000000, -27.82509854686814066, 4.525913221811051379 ) ) ;
#6335 = ORIENTED_EDGE ( 'NONE', *, *, #11225, .T. ) ;
#6336 = EDGE_LOOP ( 'NONE', ( #21615, #5565, #15308, #9420 ) ) ;
#6337 = DIRECTION ( 'NONE',  ( 0.000000000000000000, 0.000000000000000000, 1.000000000000000000 ) ) ;
#6338 = LINE ( 'NONE', #18371, #16949 ) ;
#6339 = ORIENTED_EDGE ( 'NONE', *, *, #20674, .T. ) ;
#6340 = DIRECTION ( 'NONE',  ( -1.000000000000000000, -0.000000000000000000, -0.000000000000000000 ) ) ;
#6341 = VERTEX_POINT ( 'NONE', #10345 ) ;
#6342 = EDGE_LOOP ( 'NONE', ( #20723, #16642, #12648, #21609 ) ) ;
#6343 = DIRECTION ( 'NONE',  ( 0.000000000000000000, 1.000000000000000000, 0.000000000000000000 ) ) ;
#6344 = AXIS2_PLACEMENT_3D ( 'NONE', #19262, #8483, #12109 ) ;
#6345 = DIRECTION ( 'NONE',  ( 0.000000000000000000, 0.000000000000000000, -1.000000000000000000 ) ) ;
#6346 = VERTEX_POINT ( 'NONE', #5382 ) ;
#6347 = VECTOR ( 'NONE', #12418, 1000.000000000000000 ) ;
#6348 = ORIENTED_EDGE ( 'NONE', *, *, #21178, .F. ) ;
#6349 = LINE ( 'NONE', #4454, #9661 ) ;
#6350 = AXIS2_PLACEMENT_3D ( 'NONE', #4163, #7151, #20630 ) ;
#6351 = CARTESIAN_POINT ( 'NONE',  ( -8.000000000000007105, 1.284654492305574008E-14, 104.9000000000000341 ) ) ;
#6352 = DIRECTION ( 'NONE',  ( 0.000000000000000000, 0.000000000000000000, 1.000000000000000000 ) ) ;
#6353 = DIRECTION ( 'NONE',  ( 1.000000000000000000, 0.000000000000000000, 0.000000000000000000 ) ) ;
#6354 = EDGE_CURVE ( 'NONE', #6719, #19647, #2171, .T. ) ;
#6355 = CARTESIAN_POINT ( 'NONE',  ( 10.00000000000000000, 77.39385041987100067, 35.28996114464738554 ) ) ;
#6356 = DIRECTION ( 'NONE',  ( 1.000000000000000000, 0.000000000000000000, 0.000000000000000000 ) ) ;
#6357 = PLANE ( 'NONE',  #6507 ) ;
#6358 = FACE_OUTER_BOUND ( 'NONE', #20245, .T. ) ;
#6359 = CARTESIAN_POINT ( 'NONE',  ( 10.00000000000000000, -60.65655256511276860, 59.63197188857500919 ) ) ;
#6360 = EDGE_LOOP ( 'NONE', ( #7528, #6502, #14661, #4947 ) ) ;
#6361 = EDGE_CURVE ( 'NONE', #508, #791, #17097, .T. ) ;
#6362 = ORIENTED_EDGE ( 'NONE', *, *, #19758, .F. ) ;
#6363 = CIRCLE ( 'NONE', #18709, 92.50100000000000477 ) ;
#6364 = AXIS2_PLACEMENT_3D ( 'NONE', #9778, #19631, #16533 ) ;
#6365 = DIRECTION ( 'NONE',  ( -1.000000000000000000, -0.000000000000000000, 0.000000000000000000 ) ) ;
#6366 = EDGE_CURVE ( 'NONE', #15511, #5306, #12824, .T. ) ;
#6367 = CARTESIAN_POINT ( 'NONE',  ( 10.00000000000000000, 83.35585896458619004, 16.94078559807978124 ) ) ;
#6368 = LINE ( 'NONE', #4684, #208 ) ;
#6369 = EDGE_LOOP ( 'NONE', ( #20960, #10822, #17312, #6749 ) ) ;
#6370 = SURFACE_STYLE_FILL_AREA ( #8012 ) ;
#6371 = ORIENTED_EDGE ( 'NONE', *, *, #14359, .F. ) ;
#6372 = EDGE_LOOP ( 'NONE', ( #19956, #21497, #6604, #8400 ) ) ;
#6373 = EDGE_LOOP ( 'NONE', ( #19171, #4205, #13352, #17793 ) ) ;
#6374 = CARTESIAN_POINT ( 'NONE',  ( 10.00000000000000000, -27.26034713664101972, 7.182859710736059888 ) ) ;
#6375 = ORIENTED_EDGE ( 'NONE', *, *, #15106, .T. ) ;
#6376 = EDGE_CURVE ( 'NONE', #13049, #20840, #9284, .T. ) ;
#6377 = DIRECTION ( 'NONE',  ( -1.000000000000000000, -0.000000000000000000, -0.000000000000000000 ) ) ;
#6378 = CARTESIAN_POINT ( 'NONE',  ( 5.000000000000002665, -73.32282170386882569, 48.65967342042752364 ) ) ;
#6379 = EDGE_CURVE ( 'NONE', #1789, #13415, #20946, .T. ) ;
#6380 = DIRECTION ( 'NONE',  ( 0.000000000000000000, 0.000000000000000000, 1.000000000000000000 ) ) ;
#6381 = EDGE_CURVE ( 'NONE', #15480, #15273, #832, .T. ) ;
#6382 = CIRCLE ( 'NONE', #14825, 92.50100000000000477 ) ;
#6383 = CYLINDRICAL_SURFACE ( 'NONE', #18146, 32.00000000000000000 ) ;
#6384 = CARTESIAN_POINT ( 'NONE',  ( 1.500000000000000000, 15.00000000000000000, 0.000000000000000000 ) ) ;
#6385 = LINE ( 'NONE', #16529, #10965 ) ;
#6386 = UNCERTAINTY_MEASURE_WITH_UNIT (LENGTH_MEASURE( 1.000000000000000082E-05 ), #11681, 'distance_accuracy_value', 'NONE');
#6387 = EDGE_CURVE ( 'NONE', #14519, #18351, #12114, .T. ) ;
#6388 = ORIENTED_EDGE ( 'NONE', *, *, #18412, .F. ) ;
#6389 = CARTESIAN_POINT ( 'NONE',  ( 10.00000000000000000, -60.65655256511196569, -59.63197188857583342 ) ) ;
#6390 = DIRECTION ( 'NONE',  ( 0.000000000000000000, 0.5877852522924688072, 0.8090169943749505599 ) ) ;
#6391 = ORIENTED_EDGE ( 'NONE', *, *, #20113, .F. ) ;
#6392 = CARTESIAN_POINT ( 'NONE',  ( 5.000000000000000000, -65.83713140174766920, 58.39068529131174756 ) ) ;
#6393 = EDGE_CURVE ( 'NONE', #5049, #5074, #3314, .T. ) ;
#6394 = ORIENTED_EDGE ( 'NONE', *, *, #1887, .F. ) ;
#6395 = CARTESIAN_POINT ( 'NONE',  ( 0.000000000000000000, 0.000000000000000000, 0.000000000000000000 ) ) ;
#6396 = AXIS2_PLACEMENT_3D ( 'NONE', #21407, #14781, #7815 ) ;
#6397 = CARTESIAN_POINT ( 'NONE',  ( 0.000000000000000000, 0.000000000000000000, 0.000000000000000000 ) ) ;
#6398 = VERTEX_POINT ( 'NONE', #8810 ) ;
#6399 = DIRECTION ( 'NONE',  ( -1.000000000000000000, -0.000000000000000000, -0.000000000000000000 ) ) ;
#6400 = ADVANCED_FACE ( 'NONE', ( #3938 ), #2072, .F. ) ;
#6401 = VERTEX_POINT ( 'NONE', #7146 ) ;
#6402 = ORIENTED_EDGE ( 'NONE', *, *, #10568, .F. ) ;
#6403 = DIRECTION ( 'NONE',  ( 0.000000000000000000, -1.000000000000000000, 0.000000000000000000 ) ) ;
#6404 = EDGE_CURVE ( 'NONE', #393, #3324, #5494, .T. ) ;
#6405 = ORIENTED_EDGE ( 'NONE', *, *, #17842, .F. ) ;
#6406 = LINE ( 'NONE', #4839, #5622 ) ;
#6407 = CIRCLE ( 'NONE', #21557, 44.99999999999999289 ) ;
#6408 = DIRECTION ( 'NONE',  ( -1.000000000000000000, 0.000000000000000000, -0.000000000000000000 ) ) ;
#6409 = CYLINDRICAL_SURFACE ( 'NONE', #8540, 6.887500000000022382 ) ;
#6410 = DIRECTION ( 'NONE',  ( 0.000000000000000000, 0.000000000000000000, -1.000000000000000000 ) ) ;
#6411 = EDGE_CURVE ( 'NONE', #20191, #1625, #5776, .T. ) ;
#6412 = DIRECTION ( 'NONE',  ( 1.000000000000000000, 0.000000000000000000, 0.000000000000000000 ) ) ;
#6413 = CARTESIAN_POINT ( 'NONE',  ( 0.000000000000000000, 60.00000000000000000, 9.999999999999998224 ) ) ;
#6414 = STYLED_ITEM ( 'NONE', ( #19070 ), #14875 ) ;
#6415 = DIRECTION ( 'NONE',  ( 0.000000000000000000, 0.7431448254773953543, -0.6691306063588570163 ) ) ;
#6416 = DIRECTION ( 'NONE',  ( 0.000000000000000000, 0.000000000000000000, 1.000000000000000000 ) ) ;
#6417 = DIRECTION ( 'NONE',  ( -1.000000000000000000, -0.000000000000000000, 0.000000000000000000 ) ) ;
#6418 = DIRECTION ( 'NONE',  ( 0.000000000000000000, 0.000000000000000000, 1.000000000000000000 ) ) ;
#6419 = EDGE_LOOP ( 'NONE', ( #14085, #6523 ) ) ;
#6420 = VERTEX_POINT ( 'NONE', #16990 ) ;
#6421 = ADVANCED_FACE ( 'NONE', ( #1849 ), #18977, .T. ) ;
#6422 = ORIENTED_EDGE ( 'NONE', *, *, #17164, .F. ) ;
#6423 = VERTEX_POINT ( 'NONE', #515 ) ;
#6424 = EDGE_CURVE ( 'NONE', #9318, #11653, #5434, .T. ) ;
#6425 = EDGE_CURVE ( 'NONE', #13306, #14528, #5286, .T. ) ;
#6426 = ORIENTED_EDGE ( 'NONE', *, *, #8035, .F. ) ;
#6427 = DIRECTION ( 'NONE',  ( 0.000000000000000000, 0.000000000000000000, 1.000000000000000000 ) ) ;
#6428 = VERTEX_POINT ( 'NONE', #7376 ) ;
#6429 = CARTESIAN_POINT ( 'NONE',  ( -10.00000000000000000, 0.000000000000000000, 0.000000000000000000 ) ) ;
#6430 = CARTESIAN_POINT ( 'NONE',  ( 0.000000000000000000, -92.22057093985026199, -7.197311757041478408 ) ) ;
#6431 = CARTESIAN_POINT ( 'NONE',  ( 0.000000000000000000, 0.000000000000000000, 0.000000000000000000 ) ) ;
#6432 = CYLINDRICAL_SURFACE ( 'NONE', #6951, 27.49900000000000233 ) ;
#6433 = DIRECTION ( 'NONE',  ( 0.000000000000000000, 0.000000000000000000, 1.000000000000000000 ) ) ;
#6434 = LINE ( 'NONE', #14590, #13291 ) ;
#6435 = LINE ( 'NONE', #21770, #17948 ) ;
#6436 = EDGE_LOOP ( 'NONE', ( #8519, #16616, #6159, #13847 ) ) ;
#6437 = ADVANCED_BREP_SHAPE_REPRESENTATION ( '', ( #20833, #15567 ), #9570 ) ;
#6438 = CARTESIAN_POINT ( 'NONE',  ( -10.00000000000000000, 0.000000000000000000, 0.000000000000000000 ) ) ;
#6439 = ORIENTED_EDGE ( 'NONE', *, *, #7740, .F. ) ;
#6440 = ORIENTED_EDGE ( 'NONE', *, *, #5250, .T. ) ;
#6441 = CARTESIAN_POINT ( 'NONE',  ( 8.899999999999987921, 1.456105044186203057E-14, 118.9000000000000199 ) ) ;
#6442 = AXIS2_PLACEMENT_3D ( 'NONE', #2650, #9379, #16133 ) ;
#6443 = ORIENTED_EDGE ( 'NONE', *, *, #12112, .T. ) ;
#6444 = CYLINDRICAL_SURFACE ( 'NONE', #14054, 44.99999999999999289 ) ;
#6445 = EDGE_LOOP ( 'NONE', ( #10849, #21171 ) ) ;
#6446 = ORIENTED_EDGE ( 'NONE', *, *, #3134, .F. ) ;
#6447 =( REPRESENTATION_RELATIONSHIP ('NONE','NONE', #2177, #11927 ) REPRESENTATION_RELATIONSHIP_WITH_TRANSFORMATION ( #4776 )SHAPE_REPRESENTATION_RELATIONSHIP( ) );
#6448 = DIRECTION ( 'NONE',  ( 1.000000000000000000, 0.000000000000000000, 0.000000000000000000 ) ) ;
#6449 = ORIENTED_EDGE ( 'NONE', *, *, #7029, .F. ) ;
#6450 = LINE ( 'NONE', #13164, #4044 ) ;
#6451 = DIRECTION ( 'NONE',  ( -1.000000000000000000, 0.000000000000000000, 0.000000000000000000 ) ) ;
#6452 = AXIS2_PLACEMENT_3D ( 'NONE', #17365, #2010, #2219 ) ;
#6453 = CARTESIAN_POINT ( 'NONE',  ( 10.00000000000000000, -19.85071254963763465, -20.01672328094552356 ) ) ;
#6454 = DIRECTION ( 'NONE',  ( -1.000000000000000000, 0.000000000000000000, -0.000000000000000000 ) ) ;
#6455 = DIRECTION ( 'NONE',  ( -1.000000000000000000, 0.000000000000000000, 0.000000000000000000 ) ) ;
#6456 = DIRECTION ( 'NONE',  ( 0.000000000000000000, 0.000000000000000000, 1.000000000000000000 ) ) ;
#6457 = DIRECTION ( 'NONE',  ( 0.000000000000000000, 0.000000000000000000, 1.000000000000000000 ) ) ;
#6458 = DIRECTION ( 'NONE',  ( 0.000000000000000000, 0.8660254037844362651, 0.5000000000000039968 ) ) ;
#6459 = CARTESIAN_POINT ( 'NONE',  ( 150.0000507999999968, 2.828427124746190291, -1.000000000000000000 ) ) ;
#6460 = ORIENTED_EDGE ( 'NONE', *, *, #4203, .T. ) ;
#6461 = CARTESIAN_POINT ( 'NONE',  ( 10.00000000000000000, 68.93609746931237225, -54.69748134696388320 ) ) ;
#6462 = CARTESIAN_POINT ( 'NONE',  ( 10.00000000000000000, -29.47587714451095309, 82.91666097089111531 ) ) ;
#6463 = CIRCLE ( 'NONE', #2205, 11.99999999999999822 ) ;
#6464 = EDGE_LOOP ( 'NONE', ( #19906, #13958, #4742, #354 ) ) ;
#6465 = EDGE_CURVE ( 'NONE', #2214, #7364, #12126, .T. ) ;
#6466 = DIRECTION ( 'NONE',  ( 0.000000000000000000, 3.546545773108139957E-15, -1.000000000000000000 ) ) ;
#6467 = ORIENTED_EDGE ( 'NONE', *, *, #1769, .F. ) ;
#6468 = ORIENTED_EDGE ( 'NONE', *, *, #20015, .T. ) ;
#6469 = CIRCLE ( 'NONE', #3291, 6.887500000000022382 ) ;
#6470 = FACE_OUTER_BOUND ( 'NONE', #1650, .T. ) ;
#6471 = ORIENTED_EDGE ( 'NONE', *, *, #21794, .F. ) ;
#6472 = ORIENTED_EDGE ( 'NONE', *, *, #588, .F. ) ;
#6473 = CARTESIAN_POINT ( 'NONE',  ( -90.00000000000000000, 0.000000000000000000, -5.000000000000000888 ) ) ;
#6474 = DIRECTION ( 'NONE',  ( 1.000000000000000000, -0.000000000000000000, -0.000000000000000000 ) ) ;
#6475 = EDGE_CURVE ( 'NONE', #2850, #8227, #11417, .T. ) ;
#6476 = CIRCLE ( 'NONE', #8230, 100.0000000000000284 ) ;
#6477 = VERTEX_POINT ( 'NONE', #7476 ) ;
#6478 = ADVANCED_BREP_SHAPE_REPRESENTATION ( '', ( #20339, #15567 ), #14522 ) ;
#6479 = DIRECTION ( 'NONE',  ( -1.000000000000000000, 0.000000000000000000, 0.000000000000000000 ) ) ;
#6480 = DIRECTION ( 'NONE',  ( 0.000000000000000000, 0.000000000000000000, 1.000000000000000000 ) ) ;
#6481 = CARTESIAN_POINT ( 'NONE',  ( 0.000000000000000000, 84.79630770241077187, 6.691460262316813790 ) ) ;
#6482 = DIRECTION ( 'NONE',  ( -1.000000000000000000, -0.000000000000000000, -0.000000000000000000 ) ) ;
#6483 = DIRECTION ( 'NONE',  ( -1.000000000000000000, 0.000000000000000000, 0.000000000000000000 ) ) ;
#6484 = CARTESIAN_POINT ( 'NONE',  ( 1.500000000000000000, 0.000000000000000000, 5.000000000000000000 ) ) ;
#6485 = AXIS2_PLACEMENT_3D ( 'NONE', #10267, #19425, #757 ) ;
#6486 = ORIENTED_EDGE ( 'NONE', *, *, #15173, .F. ) ;
#6487 = CARTESIAN_POINT ( 'NONE',  ( -10.00000000000000000, 0.000000000000000000, 0.000000000000000000 ) ) ;
#6488 = CIRCLE ( 'NONE', #11053, 44.99999999999998579 ) ;
#6489 = DIRECTION ( 'NONE',  ( 0.000000000000000000, 0.9510565162951544194, -0.3090169943749448422 ) ) ;
#6490 = ORIENTED_EDGE ( 'NONE', *, *, #3163, .F. ) ;
#6491 = CARTESIAN_POINT ( 'NONE',  ( -10.00000000000000000, 0.000000000000000000, 0.000000000000000000 ) ) ;
#6492 = ORIENTED_EDGE ( 'NONE', *, *, #7461, .T. ) ;
#6493 = CIRCLE ( 'NONE', #2590, 92.50100000000000477 ) ;
#6494 = EDGE_CURVE ( 'NONE', #17311, #11431, #21308, .T. ) ;
#6495 = EDGE_CURVE ( 'NONE', #14735, #19098, #19888, .T. ) ;
#6496 = EDGE_CURVE ( 'NONE', #13465, #18176, #11785, .T. ) ;
#6497 = CYLINDRICAL_SURFACE ( 'NONE', #11963, 44.99999999999999289 ) ;
#6498 = ORIENTED_EDGE ( 'NONE', *, *, #5060, .T. ) ;
#6499 = CARTESIAN_POINT ( 'NONE',  ( 5.000000000000002665, 46.07110168784820559, 74.97635353408399794 ) ) ;
#6500 = EDGE_CURVE ( 'NONE', #19369, #10257, #20244, .T. ) ;
#6501 = AXIS2_PLACEMENT_3D ( 'NONE', #4932, #18515, #16411 ) ;
#6502 = ORIENTED_EDGE ( 'NONE', *, *, #5969, .T. ) ;
#6503 = VERTEX_POINT ( 'NONE', #9334 ) ;
#6504 = DIRECTION ( 'NONE',  ( -1.000000000000000000, 0.000000000000000000, -0.000000000000000000 ) ) ;
#6505 = VERTEX_POINT ( 'NONE', #737 ) ;
#6506 = DIRECTION ( 'NONE',  ( -1.000000000000000000, 0.000000000000000000, 0.000000000000000000 ) ) ;
#6507 = AXIS2_PLACEMENT_3D ( 'NONE', #6242, #1368, #6457 ) ;
#6508 = DIRECTION ( 'NONE',  ( 0.000000000000000000, 0.000000000000000000, 1.000000000000000000 ) ) ;
#6509 = CARTESIAN_POINT ( 'NONE',  ( -1.500000000000001332, 8.239576745513313235E-16, 6.728125000000022560 ) ) ;
#6510 = LINE ( 'NONE', #10133, #17812 ) ;
#6511 = PRODUCT_DEFINITION_SHAPE ( 'NONE', 'NONE',  #21862 ) ;
#6512 = DIRECTION ( 'NONE',  ( 0.000000000000000000, 0.9945218953682729568, 0.1045284632676570374 ) ) ;
#6513 = CIRCLE ( 'NONE', #4379, 44.99999999999998579 ) ;
#6514 = EDGE_CURVE ( 'NONE', #14098, #13007, #2499, .T. ) ;
#6515 = CARTESIAN_POINT ( 'NONE',  ( -10.00000000000000000, 0.000000000000000000, 0.000000000000000000 ) ) ;
#6516 = DIRECTION ( 'NONE',  ( 0.000000000000000000, 0.000000000000000000, 1.000000000000000000 ) ) ;
#6517 = EDGE_CURVE ( 'NONE', #17888, #9822, #10705, .T. ) ;
#6518 = DIRECTION ( 'NONE',  ( 0.000000000000000000, 0.000000000000000000, -1.000000000000000000 ) ) ;
#6519 = AXIS2_PLACEMENT_3D ( 'NONE', #5359, #60, #3695 ) ;
#6520 = CARTESIAN_POINT ( 'NONE',  ( 10.00000000000000000, 5.479102470010468018, 87.82926298292115064 ) ) ;
#6521 = CARTESIAN_POINT ( 'NONE',  ( -10.00000000000000000, 0.000000000000000000, 0.000000000000000000 ) ) ;
#6522 = CIRCLE ( 'NONE', #6171, 44.99999999999999289 ) ;
#6523 = ORIENTED_EDGE ( 'NONE', *, *, #10122, .F. ) ;
#6524 = ORIENTED_EDGE ( 'NONE', *, *, #3112, .T. ) ;
#6525 = AXIS2_PLACEMENT_3D ( 'NONE', #5785, #12507, #19259 ) ;
#6526 = VERTEX_POINT ( 'NONE', #4490 ) ;
#6527 = EDGE_CURVE ( 'NONE', #5809, #7682, #13534, .T. ) ;
#6528 = ORIENTED_EDGE ( 'NONE', *, *, #1892, .T. ) ;
#6529 = ORIENTED_EDGE ( 'NONE', *, *, #18834, .F. ) ;
#6530 = CYLINDRICAL_SURFACE ( 'NONE', #21469, 5.612499999999999822 ) ;
#6531 = AXIS2_PLACEMENT_3D ( 'NONE', #14837, #21578, #6456 ) ;
#6532 = ORIENTED_EDGE ( 'NONE', *, *, #6424, .T. ) ;
#6533 = CARTESIAN_POINT ( 'NONE',  ( 0.000000000000000000, 0.000000000000000000, 0.000000000000000000 ) ) ;
#6534 = AXIS2_PLACEMENT_3D ( 'NONE', #14679, #13453, #6741 ) ;
#6535 = CIRCLE ( 'NONE', #3694, 3.000000000000000444 ) ;
#6536 = FACE_OUTER_BOUND ( 'NONE', #3374, .T. ) ;
#6537 = EDGE_CURVE ( 'NONE', #16339, #10824, #18129, .T. ) ;
#6538 = CIRCLE ( 'NONE', #8629, 44.99999999999999289 ) ;
#6539 = CARTESIAN_POINT ( 'NONE',  ( -10.00000000000000000, 0.000000000000000000, 0.000000000000000000 ) ) ;
#6540 = CARTESIAN_POINT ( 'NONE',  ( 10.00000000000000000, 25.17124263951009411, -12.69364185792227495 ) ) ;
#6541 = DIRECTION ( 'NONE',  ( 0.000000000000000000, -1.000000000000000000, 0.000000000000000000 ) ) ;
#6542 = EDGE_CURVE ( 'NONE', #17273, #6557, #14946, .T. ) ;
#6543 = CIRCLE ( 'NONE', #13588, 88.00000000000000000 ) ;
#6544 = DIRECTION ( 'NONE',  ( 0.000000000000000000, 0.000000000000000000, 1.000000000000000000 ) ) ;
#6545 = CARTESIAN_POINT ( 'NONE',  ( 0.000000000000000000, 81.55207211302078463, -24.17537951050094236 ) ) ;
#6546 = EDGE_CURVE ( 'NONE', #16218, #8158, #19538, .T. ) ;
#6547 = VERTEX_POINT ( 'NONE', #17978 ) ;
#6548 = EDGE_CURVE ( 'NONE', #7517, #16720, #4001, .T. ) ;
#6549 = CARTESIAN_POINT ( 'NONE',  ( 10.00000000000000000, 2.481790431839256517, 92.46770094066594936 ) ) ;
#6550 = AXIS2_PLACEMENT_3D ( 'NONE', #13431, #1407, #1294 ) ;
#6551 = ORIENTED_EDGE ( 'NONE', *, *, #21621, .T. ) ;
#6552 = AXIS2_PLACEMENT_3D ( 'NONE', #8699, #307, #10572 ) ;
#6553 = ORIENTED_EDGE ( 'NONE', *, *, #19852, .F. ) ;
#6554 = CIRCLE ( 'NONE', #11834, 3.000000000000000444 ) ;
#6555 = DIRECTION ( 'NONE',  ( -1.000000000000000000, 0.000000000000000000, 0.000000000000000000 ) ) ;
#6556 = EDGE_CURVE ( 'NONE', #14635, #18240, #16349, .T. ) ;
#6557 = VERTEX_POINT ( 'NONE', #21062 ) ;
#6558 = DIRECTION ( 'NONE',  ( -1.000000000000000000, -0.000000000000000000, 0.000000000000000000 ) ) ;
#6559 = ORIENTED_EDGE ( 'NONE', *, *, #16071, .F. ) ;
#6560 = ORIENTED_EDGE ( 'NONE', *, *, #5005, .F. ) ;
#6561 = AXIS2_PLACEMENT_3D ( 'NONE', #14788, #14890, #4724 ) ;
#6562 = ITEM_DEFINED_TRANSFORMATION ( 'NONE', 'NONE', #11706,  #15567 ) ;
#6563 = LINE ( 'NONE', #14933, #4520 ) ;
#6564 = ORIENTED_EDGE ( 'NONE', *, *, #12403, .T. ) ;
#6565 = AXIS2_PLACEMENT_3D ( 'NONE', #13751, #2141, #18730 ) ;
#6566 = CARTESIAN_POINT ( 'NONE',  ( -7.500000000000000000, 0.000000000000000000, 3.000000000000000000 ) ) ;
#6567 = LINE ( 'NONE', #3224, #12077 ) ;
#6568 = DIRECTION ( 'NONE',  ( 1.000000000000000000, 0.000000000000000000, 0.000000000000000000 ) ) ;
#6569 = CARTESIAN_POINT ( 'NONE',  ( 10.00000000000000000, 36.60317927562579854, 76.78148674856777234 ) ) ;
#6570 = CIRCLE ( 'NONE', #12192, 92.50099999999999056 ) ;
#6571 = AXIS2_PLACEMENT_3D ( 'NONE', #15274, #46, #10414 ) ;
#6572 = CIRCLE ( 'NONE', #11145, 44.99999999999999289 ) ;
#6573 = DIRECTION ( 'NONE',  ( -0.000000000000000000, -0.000000000000000000, 1.000000000000000000 ) ) ;
#6574 = FACE_OUTER_BOUND ( 'NONE', #19364, .T. ) ;
#6575 = CARTESIAN_POINT ( 'NONE',  ( 0.000000000000000000, -16.79755869217588682, -90.96305306542271296 ) ) ;
#6576 = VERTEX_POINT ( 'NONE', #15879 ) ;
#6577 = DIRECTION ( 'NONE',  ( 0.000000000000000000, 0.000000000000000000, 1.000000000000000000 ) ) ;
#6578 = DIRECTION ( 'NONE',  ( 1.000000000000000000, 0.000000000000000000, 0.000000000000000000 ) ) ;
#6579 = ORIENTED_EDGE ( 'NONE', *, *, #16759, .T. ) ;
#6580 = AXIS2_PLACEMENT_3D ( 'NONE', #13817, #235, #7091 ) ;
#6581 = LINE ( 'NONE', #8333, #21013 ) ;
#6582 = ORIENTED_EDGE ( 'NONE', *, *, #18382, .T. ) ;
#6583 = CIRCLE ( 'NONE', #16090, 92.50100000000000477 ) ;
#6584 = AXIS2_PLACEMENT_3D ( 'NONE', #9380, #5059, #1424 ) ;
#6585 = EDGE_LOOP ( 'NONE', ( #16984, #14881, #19356, #6230 ) ) ;
#6586 = CARTESIAN_POINT ( 'NONE',  ( 10.00000000000000000, 7.240962358591573889, 31.16999300804317130 ) ) ;
#6587 = ORIENTED_EDGE ( 'NONE', *, *, #3774, .F. ) ;
#6588 = VERTEX_POINT ( 'NONE', #5930 ) ;
#6589 = CARTESIAN_POINT ( 'NONE',  ( 10.00000000000000000, 18.94217447942559573, 85.93715160505956874 ) ) ;
#6590 = DIRECTION ( 'NONE',  ( 0.000000000000000000, -0.2756373558169869509, -0.9612616959383223358 ) ) ;
#6591 = ORIENTED_EDGE ( 'NONE', *, *, #13411, .T. ) ;
#6592 = DIRECTION ( 'NONE',  ( 0.000000000000000000, 0.000000000000000000, 1.000000000000000000 ) ) ;
#6593 = DIRECTION ( 'NONE',  ( 0.000000000000000000, -0.4694715627858975782, 0.8829475928589234357 ) ) ;
#6594 = DIRECTION ( 'NONE',  ( 0.000000000000000000, 1.224646799147322392E-16, 1.000000000000000000 ) ) ;
#6595 = DIRECTION ( 'NONE',  ( -0.000000000000000000, -0.000000000000000000, 1.000000000000000000 ) ) ;
#6596 = PLANE ( 'NONE',  #17058 ) ;
#6597 = CARTESIAN_POINT ( 'NONE',  ( 5.000000000000000000, 5.000000000000000000, 9.999999999999998224 ) ) ;
#6598 = EDGE_CURVE ( 'NONE', #3581, #2939, #4159, .T. ) ;
#6599 = AXIS2_PLACEMENT_3D ( 'NONE', #15654, #14000, #526 ) ;
#6600 = ORIENTED_EDGE ( 'NONE', *, *, #597, .F. ) ;
#6601 = AXIS2_PLACEMENT_3D ( 'NONE', #19674, #11379, #4544 ) ;
#6602 = CARTESIAN_POINT ( 'NONE',  ( 10.00000000000000000, 0.000000000000000000, 0.000000000000000000 ) ) ;
#6603 = CYLINDRICAL_SURFACE ( 'NONE', #4435, 92.50100000000000477 ) ;
#6604 = ORIENTED_EDGE ( 'NONE', *, *, #15247, .T. ) ;
#6605 = PRODUCT_RELATED_PRODUCT_CATEGORY ( 'part', '', ( #9642 ) ) ;
#6606 = CARTESIAN_POINT ( 'NONE',  ( 10.00000000000000000, 52.96496548042942010, -66.55750800669305534 ) ) ;
#6607 = VERTEX_POINT ( 'NONE', #19183 ) ;
#6608 = DIRECTION ( 'NONE',  ( 1.000000000000000000, -0.000000000000000000, 0.000000000000000000 ) ) ;
#6609 = DIRECTION ( 'NONE',  ( 0.000000000000000000, 0.000000000000000000, 1.000000000000000000 ) ) ;
#6610 = ORIENTED_EDGE ( 'NONE', *, *, #17422, .F. ) ;
#6611 = DIRECTION ( 'NONE',  ( 0.000000000000000000, 0.000000000000000000, 1.000000000000000000 ) ) ;
#6612 = VECTOR ( 'NONE', #11714, 1000.000000000000000 ) ;
#6613 = VERTEX_POINT ( 'NONE', #4267 ) ;
#6614 = AXIS2_PLACEMENT_3D ( 'NONE', #4943, #18320, #1296 ) ;
#6615 = VERTEX_POINT ( 'NONE', #4043 ) ;
#6616 = DIRECTION ( 'NONE',  ( -1.000000000000000000, -0.000000000000000000, -0.000000000000000000 ) ) ;
#6617 = CIRCLE ( 'NONE', #9774, 45.00000000000000000 ) ;
#6618 = VERTEX_POINT ( 'NONE', #17649 ) ;
#6619 = DIRECTION ( 'NONE',  ( -1.000000000000000000, -0.000000000000000000, -0.000000000000000000 ) ) ;
#6620 = DIRECTION ( 'NONE',  ( -1.000000000000000000, -0.000000000000000000, -0.000000000000000000 ) ) ;
#6621 = CARTESIAN_POINT ( 'NONE',  ( 0.000000000000000000, 29.47587714451039531, 82.91666097089130005 ) ) ;
#6622 = DIRECTION ( 'NONE',  ( 0.000000000000000000, -0.9945218953682744001, 0.1045284632676437286 ) ) ;
#6623 = DIRECTION ( 'NONE',  ( 1.000000000000000000, 0.000000000000000000, 0.000000000000000000 ) ) ;
#6624 = EDGE_CURVE ( 'NONE', #18366, #6894, #4717, .T. ) ;
#6625 = DIRECTION ( 'NONE',  ( -1.000000000000000000, -0.000000000000000000, -0.000000000000000000 ) ) ;
#6626 = CARTESIAN_POINT ( 'NONE',  ( -9.999999999999998224, 0.000000000000000000, 15.00000000000000000 ) ) ;
#6627 = DIRECTION ( 'NONE',  ( -1.000000000000000000, 0.000000000000000000, 0.000000000000000000 ) ) ;
#6628 = VECTOR ( 'NONE', #14530, 1000.000000000000000 ) ;
#6629 = DIRECTION ( 'NONE',  ( 0.000000000000000000, 0.000000000000000000, -1.000000000000000000 ) ) ;
#6630 = CIRCLE ( 'NONE', #18263, 11.99999999999999822 ) ;
#6631 = VECTOR ( 'NONE', #6182, 1000.000000000000000 ) ;
#6632 = FACE_OUTER_BOUND ( 'NONE', #932, .T. ) ;
#6633 = ORIENTED_EDGE ( 'NONE', *, *, #12154, .T. ) ;
#6634 = CARTESIAN_POINT ( 'NONE',  ( 0.000000000000000000, 0.000000000000000000, 0.000000000000000000 ) ) ;
#6635 = ORIENTED_EDGE ( 'NONE', *, *, #9479, .T. ) ;
#6636 = ORIENTED_EDGE ( 'NONE', *, *, #3608, .F. ) ;
#6637 = EDGE_CURVE ( 'NONE', #18968, #5218, #14430, .T. ) ;
#6638 = VERTEX_POINT ( 'NONE', #9655 ) ;
#6639 = VERTEX_POINT ( 'NONE', #3258 ) ;
#6640 = EDGE_CURVE ( 'NONE', #4926, #4858, #12470, .T. ) ;
#6641 = CARTESIAN_POINT ( 'NONE',  ( 0.000000000000000000, -74.74361964203200159, -40.60271866773624083 ) ) ;
#6642 = AXIS2_PLACEMENT_3D ( 'NONE', #15963, #11401, #1456 ) ;
#6643 = ORIENTED_EDGE ( 'NONE', *, *, #6078, .F. ) ;
#6644 = CARTESIAN_POINT ( 'NONE',  ( 10.00000000000000000, -90.63195040374199607, 18.50093422002390398 ) ) ;
#6645 = VECTOR ( 'NONE', #19945, 1000.000000000000000 ) ;
#6646 = VECTOR ( 'NONE', #1693, 1000.000000000000000 ) ;
#6647 = DIRECTION ( 'NONE',  ( 0.000000000000000000, 0.000000000000000000, -1.000000000000000000 ) ) ;
#6648 = EDGE_CURVE ( 'NONE', #4047, #839, #17072, .T. ) ;
#6649 = LINE ( 'NONE', #15345, #7169 ) ;
#6650 = EDGE_CURVE ( 'NONE', #13109, #14874, #7534, .T. ) ;
#6651 = CYLINDRICAL_SURFACE ( 'NONE', #4491, 92.50100000000000477 ) ;
#6652 = ADVANCED_FACE ( 'NONE', ( #21823 ), #11326, .F. ) ;
#6653 = DIRECTION ( 'NONE',  ( -1.000000000000000000, 0.000000000000000000, -0.000000000000000000 ) ) ;
#6654 = CIRCLE ( 'NONE', #18993, 32.00000000000000000 ) ;
#6655 = PLANE ( 'NONE',  #9820 ) ;
#6656 = EDGE_CURVE ( 'NONE', #826, #1308, #8347, .T. ) ;
#6657 = VERTEX_POINT ( 'NONE', #13312 ) ;
#6658 = CARTESIAN_POINT ( 'NONE',  ( 10.00000000000000000, 57.47876254627143311, 62.70072803846409215 ) ) ;
#6659 = AXIS2_PLACEMENT_3D ( 'NONE', #2436, #9377, #7743 ) ;
#6660 = AXIS2_PLACEMENT_3D ( 'NONE', #3788, #13838, #15169 ) ;
#6661 = VERTEX_POINT ( 'NONE', #21601 ) ;
#6662 = CIRCLE ( 'NONE', #8771, 44.99999999999999289 ) ;
#6663 = CIRCLE ( 'NONE', #2767, 88.00000000000000000 ) ;
#6664 = ORIENTED_EDGE ( 'NONE', *, *, #12685, .T. ) ;
#6665 = EDGE_CURVE ( 'NONE', #9782, #628, #7198, .T. ) ;
#6666 = CARTESIAN_POINT ( 'NONE',  ( 0.000000000000000000, -23.57863763525709189, -15.45211464167688753 ) ) ;
#6667 = ORIENTED_EDGE ( 'NONE', *, *, #6275, .T. ) ;
#6668 = DIRECTION ( 'NONE',  ( -1.000000000000000000, -0.000000000000000000, 0.000000000000000000 ) ) ;
#6669 = ORIENTED_EDGE ( 'NONE', *, *, #4206, .T. ) ;
#6670 = EDGE_CURVE ( 'NONE', #19369, #17019, #1605, .T. ) ;
#6671 = ORIENTED_EDGE ( 'NONE', *, *, #21697, .T. ) ;
#6672 = ITEM_DEFINED_TRANSFORMATION ( 'NONE', 'NONE', #8871,  #15567 ) ;
#6673 = EDGE_CURVE ( 'NONE', #10108, #1056, #2930, .T. ) ;
#6674 = CYLINDRICAL_SURFACE ( 'NONE', #15799, 88.00000000000000000 ) ;
#6675 = VERTEX_POINT ( 'NONE', #6270 ) ;
#6676 = CARTESIAN_POINT ( 'NONE',  ( -10.00000000000000000, 0.000000000000000000, 0.000000000000000000 ) ) ;
#6677 = CARTESIAN_POINT ( 'NONE',  ( 10.00000000000000000, -79.38136668499713267, -37.98155635597392887 ) ) ;
#6678 = EDGE_CURVE ( 'NONE', #10690, #16223, #11432, .T. ) ;
#6679 = AXIS2_PLACEMENT_3D ( 'NONE', #13464, #5081, #222 ) ;
#6680 = DIRECTION ( 'NONE',  ( 0.000000000000000000, 0.000000000000000000, -1.000000000000000000 ) ) ;
#6681 = FACE_OUTER_BOUND ( 'NONE', #9646, .T. ) ;
#6682 = CIRCLE ( 'NONE', #1013, 5.633200000000004870 ) ;
#6683 = DIRECTION ( 'NONE',  ( 0.000000000000000000, 0.000000000000000000, 1.000000000000000000 ) ) ;
#6684 = AXIS2_PLACEMENT_3D ( 'NONE', #5682, #12408, #1826 ) ;
#6685 = CIRCLE ( 'NONE', #4550, 44.99999999999999289 ) ;
#6686 = DIRECTION ( 'NONE',  ( 0.000000000000000000, 0.000000000000000000, 1.000000000000000000 ) ) ;
#6687 = PLANE ( 'NONE',  #8328 ) ;
#6688 = CARTESIAN_POINT ( 'NONE',  ( 10.00000000000000000, -15.32665449651985590, 91.22241316115413667 ) ) ;
#6689 = EDGE_CURVE ( 'NONE', #3682, #12864, #12141, .T. ) ;
#6690 = VERTEX_POINT ( 'NONE', #12987 ) ;
#6691 = EDGE_CURVE ( 'NONE', #11054, #6401, #18508, .T. ) ;
#6692 = CARTESIAN_POINT ( 'NONE',  ( 0.000000000000000000, 100.0000000000000000, 0.000000000000000000 ) ) ;
#6693 = AXIS2_PLACEMENT_3D ( 'NONE', #7994, #1248, #10969 ) ;
#6694 = DIRECTION ( 'NONE',  ( -0.000000000000000000, -0.000000000000000000, 1.000000000000000000 ) ) ;
#6695 = ORIENTED_EDGE ( 'NONE', *, *, #8946, .T. ) ;
#6696 = AXIS2_PLACEMENT_3D ( 'NONE', #9670, #8042, #20081 ) ;
#6697 = VECTOR ( 'NONE', #7922, 1000.000000000000000 ) ;
#6698 = DIRECTION ( 'NONE',  ( 1.000000000000000000, 0.000000000000000000, 0.000000000000000000 ) ) ;
#6699 = EDGE_CURVE ( 'NONE', #12588, #21211, #15674, .T. ) ;
#6700 = PRODUCT_DEFINITION_SHAPE ( 'NONE', 'NONE',  #21861 ) ;
#6701 = EDGE_LOOP ( 'NONE', ( #3107, #12661, #9824, #3435 ) ) ;
#6702 = ORIENTED_EDGE ( 'NONE', *, *, #20822, .F. ) ;
#6703 = DIRECTION ( 'NONE',  ( 1.000000000000000000, 0.000000000000000000, 0.000000000000000000 ) ) ;
#6704 = ORIENTED_EDGE ( 'NONE', *, *, #15582, .F. ) ;
#6705 = VERTEX_POINT ( 'NONE', #18191 ) ;
#6706 = LINE ( 'NONE', #11661, #3723 ) ;
#6707 = ORIENTED_EDGE ( 'NONE', *, *, #2998, .T. ) ;
#6708 = ADVANCED_FACE ( 'NONE', ( #14761 ), #6383, .T. ) ;
#6709 = CARTESIAN_POINT ( 'NONE',  ( 0.000000000000000000, -10.41137886060169038, 91.91321010181843576 ) ) ;
#6710 = DIRECTION ( 'NONE',  ( 1.000000000000000000, 0.000000000000000000, 0.000000000000000000 ) ) ;
#6711 = CARTESIAN_POINT ( 'NONE',  ( 10.00000000000000000, 14.53731623274928708, 23.34226719384910709 ) ) ;
#6712 = DIRECTION ( 'NONE',  ( 0.000000000000000000, 0.000000000000000000, 1.000000000000000000 ) ) ;
#6713 = CARTESIAN_POINT ( 'NONE',  ( -10.00000000000000000, 0.000000000000000000, 0.000000000000000000 ) ) ;
#6714 = CARTESIAN_POINT ( 'NONE',  ( -90.00000000000000000, 0.000000000000000000, 0.000000000000000000 ) ) ;
#6715 = AXIS2_PLACEMENT_3D ( 'NONE', #16163, #9406, #11189 ) ;
#6716 = VERTEX_POINT ( 'NONE', #14867 ) ;
#6717 = DIRECTION ( 'NONE',  ( 0.000000000000000000, 0.000000000000000000, 1.000000000000000000 ) ) ;
#6718 = CARTESIAN_POINT ( 'NONE',  ( 10.00000000000000000, 60.65279801375343993, 63.75921967137637836 ) ) ;
#6719 = VERTEX_POINT ( 'NONE', #4815 ) ;
#6720 = FACE_OUTER_BOUND ( 'NONE', #12205, .T. ) ;
#6721 = SHAPE_REPRESENTATION ( 'internal spur gear_iso_ISO - Internal spur gear 2M 90T 20PA 10FW ---S90S200OD 1.0AF', ( #15567 ), #19793 ) ;
#6722 = ORIENTED_EDGE ( 'NONE', *, *, #7235, .F. ) ;
#6723 = CYLINDRICAL_SURFACE ( 'NONE', #21489, 27.49900000000000233 ) ;
#6724 = EDGE_CURVE ( 'NONE', #2060, #2109, #14249, .T. ) ;
#6725 = ORIENTED_EDGE ( 'NONE', *, *, #18657, .T. ) ;
#6726 = CARTESIAN_POINT ( 'NONE',  ( 0.000000000000000000, 0.000000000000000000, -3.000000000000000000 ) ) ;
#6727 = ORIENTED_EDGE ( 'NONE', *, *, #2848, .T. ) ;
#6728 = ORIENTED_EDGE ( 'NONE', *, *, #1781, .T. ) ;
#6729 = VERTEX_POINT ( 'NONE', #8235 ) ;
#6730 = AXIS2_PLACEMENT_3D ( 'NONE', #16717, #5011, #15170 ) ;
#6731 = CARTESIAN_POINT ( 'NONE',  ( 0.000000000000000000, -84.79630770241089976, 6.691460262315113816 ) ) ;
#6732 = VERTEX_POINT ( 'NONE', #14966 ) ;
#6733 = FACE_OUTER_BOUND ( 'NONE', #11550, .T. ) ;
#6734 = DIRECTION ( 'NONE',  ( 0.000000000000000000, 0.9510565162951544194, -0.3090169943749449533 ) ) ;
#6735 = DIRECTION ( 'NONE',  ( 0.000000000000000000, 0.000000000000000000, 1.000000000000000000 ) ) ;
#6736 = DIRECTION ( 'NONE',  ( 0.000000000000000000, 0.000000000000000000, 1.000000000000000000 ) ) ;
#6737 = CARTESIAN_POINT ( 'NONE',  ( 0.000000000000000000, 0.000000000000000000, 3.000000000000000000 ) ) ;
#6738 = CARTESIAN_POINT ( 'NONE',  ( 1.500000000000001332, 0.000000000000000000, 0.000000000000000000 ) ) ;
#6739 = CARTESIAN_POINT ( 'NONE',  ( 10.00000000000000000, -64.95266917914277371, -59.37298010463037912 ) ) ;
#6740 = CARTESIAN_POINT ( 'NONE',  ( 10.00000000000000000, -78.04699792498179534, 49.64978465107262906 ) ) ;
#6741 = DIRECTION ( 'NONE',  ( 0.000000000000000000, -1.063963731932441790E-14, -1.000000000000000000 ) ) ;
#6742 = CIRCLE ( 'NONE', #16245, 45.00000000000000000 ) ;
#6743 = DIRECTION ( 'NONE',  ( -1.000000000000000000, 0.000000000000000000, -0.000000000000000000 ) ) ;
#6744 = ORIENTED_EDGE ( 'NONE', *, *, #7312, .T. ) ;
#6745 = DIRECTION ( 'NONE',  ( 1.000000000000000000, 0.000000000000000000, 0.000000000000000000 ) ) ;
#6746 = ORIENTED_EDGE ( 'NONE', *, *, #2532, .F. ) ;
#6747 = PLANE ( 'NONE',  #7360 ) ;
#6748 = ORIENTED_EDGE ( 'NONE', *, *, #20288, .F. ) ;
#6749 = ORIENTED_EDGE ( 'NONE', *, *, #7306, .F. ) ;
#6750 = EDGE_CURVE ( 'NONE', #3104, #2973, #4733, .T. ) ;
#6751 = ORIENTED_EDGE ( 'NONE', *, *, #7928, .F. ) ;
#6752 = CARTESIAN_POINT ( 'NONE',  ( -7.500000000000000000, 0.000000000000000000, 3.000000000000000000 ) ) ;
#6753 = ORIENTED_EDGE ( 'NONE', *, *, #17310, .T. ) ;
#6754 = CARTESIAN_POINT ( 'NONE',  ( 0.000000000000000000, -52.34334029047928993, 76.26670130689468863 ) ) ;
#6755 = DIRECTION ( 'NONE',  ( -1.000000000000000000, -0.000000000000000000, -0.000000000000000000 ) ) ;
#6756 = EDGE_CURVE ( 'NONE', #12590, #8355, #11667, .T. ) ;
#6757 = DIRECTION ( 'NONE',  ( 0.000000000000000000, 0.000000000000000000, 1.000000000000000000 ) ) ;
#6758 = CARTESIAN_POINT ( 'NONE',  ( 10.00000000000000000, 26.27606311335951617, 10.21217444509420424 ) ) ;
#6759 = CARTESIAN_POINT ( 'NONE',  ( 0.000000000000000000, 90.32141448704683739, 19.96189084378252332 ) ) ;
#6760 = EDGE_CURVE ( 'NONE', #20731, #14184, #17792, .T. ) ;
#6761 = FACE_OUTER_BOUND ( 'NONE', #4469, .T. ) ;
#6762 = ORIENTED_EDGE ( 'NONE', *, *, #11821, .T. ) ;
#6763 = CARTESIAN_POINT ( 'NONE',  ( 0.000000000000000000, 2.481790431840498634, -92.46770094066590673 ) ) ;
#6764 = VERTEX_POINT ( 'NONE', #12310 ) ;
#6765 = VERTEX_POINT ( 'NONE', #6807 ) ;
#6766 = CARTESIAN_POINT ( 'NONE',  ( 10.00000000000000000, -52.96496548042899377, 66.55750800669339640 ) ) ;
#6767 = ADVANCED_FACE ( 'NONE', ( #12202 ), #6917, .T. ) ;
#6768 = ORIENTED_EDGE ( 'NONE', *, *, #1618, .T. ) ;
#6769 = ADVANCED_FACE ( 'NONE', ( #20392 ), #10430, .F. ) ;
#6770 = ADVANCED_FACE ( 'NONE', ( #5254 ), #13530, .F. ) ;
#6771 = CARTESIAN_POINT ( 'NONE',  ( 10.00000000000000000, -15.25521607131190294, -23.70650506194185425 ) ) ;
#6772 = VERTEX_POINT ( 'NONE', #18626 ) ;
#6773 = ORIENTED_EDGE ( 'NONE', *, *, #7327, .T. ) ;
#6774 = SHAPE_DEFINITION_REPRESENTATION ( #13742, #11927 ) ;
#6775 = FACE_OUTER_BOUND ( 'NONE', #1761, .T. ) ;
#6776 = EDGE_CURVE ( 'NONE', #15522, #18255, #3806, .T. ) ;
#6777 = VERTEX_POINT ( 'NONE', #3483 ) ;
#6778 = CARTESIAN_POINT ( 'NONE',  ( 0.000000000000000000, -92.32475887865419395, -5.707354816231489991 ) ) ;
#6779 = PLANE ( 'NONE',  #5485 ) ;
#6780 = CARTESIAN_POINT ( 'NONE',  ( 10.00000000000000000, 91.49386717542239467, -13.61276130276895557 ) ) ;
#6781 = DIRECTION ( 'NONE',  ( -1.000000000000000000, 0.000000000000000000, 0.000000000000000000 ) ) ;
#6782 = DIRECTION ( 'NONE',  ( -1.000000000000000000, -0.000000000000000000, -0.000000000000000000 ) ) ;
#6783 = DIRECTION ( 'NONE',  ( -1.000000000000000000, -0.000000000000000000, -0.000000000000000000 ) ) ;
#6784 = EDGE_CURVE ( 'NONE', #10646, #17995, #10220, .T. ) ;
#6785 = CARTESIAN_POINT ( 'NONE',  ( 10.00000000000000000, 0.000000000000000000, 0.000000000000000000 ) ) ;
#6786 = ORIENTED_EDGE ( 'NONE', *, *, #15389, .F. ) ;
#6787 = VECTOR ( 'NONE', #4725, 1000.000000000000000 ) ;
#6788 = EDGE_CURVE ( 'NONE', #18503, #628, #16966, .T. ) ;
#6789 = CARTESIAN_POINT ( 'NONE',  ( 0.000000000000000000, 0.000000000000000000, -3.000000000000000000 ) ) ;
#6790 = CARTESIAN_POINT ( 'NONE',  ( 1.139999999999998570, 0.000000000000000000, -6.866799999999992465 ) ) ;
#6791 = ORIENTED_EDGE ( 'NONE', *, *, #7529, .T. ) ;
#6792 = FACE_OUTER_BOUND ( 'NONE', #17114, .T. ) ;
#6793 = ORIENTED_EDGE ( 'NONE', *, *, #21763, .T. ) ;
#6794 = ORIENTED_EDGE ( 'NONE', *, *, #12154, .F. ) ;
#6795 = CARTESIAN_POINT ( 'NONE',  ( -8.900000000000019895, 0.000000000000000000, 0.000000000000000000 ) ) ;
#6796 = EDGE_CURVE ( 'NONE', #14440, #13819, #17069, .T. ) ;
#6797 = VECTOR ( 'NONE', #13281, 1000.000000000000000 ) ;
#6798 = ORIENTED_EDGE ( 'NONE', *, *, #17407, .F. ) ;
#6799 = ORIENTED_EDGE ( 'NONE', *, *, #5, .F. ) ;
#6800 = LINE ( 'NONE', #20492, #17445 ) ;
#6801 = DIRECTION ( 'NONE',  ( 0.000000000000000000, 0.000000000000000000, 1.000000000000000000 ) ) ;
#6802 = ORIENTED_EDGE ( 'NONE', *, *, #1624, .F. ) ;
#6803 = AXIS2_PLACEMENT_3D ( 'NONE', #14368, #13038, #16462 ) ;
#6804 = DIRECTION ( 'NONE',  ( 0.000000000000000000, -0.9510565162951566398, 0.3090169943749382364 ) ) ;
#6805 = DIRECTION ( 'NONE',  ( 0.000000000000000000, 0.000000000000000000, -1.000000000000000000 ) ) ;
#6806 = CARTESIAN_POINT ( 'NONE',  ( 10.00000000000000000, 0.000000000000000000, 0.000000000000000000 ) ) ;
#6807 = CARTESIAN_POINT ( 'NONE',  ( 0.000000000000000000, -8.925965667929483871, 92.06933331948778232 ) ) ;
#6808 = CIRCLE ( 'NONE', #786, 88.00000000000000000 ) ;
#6809 = DIRECTION ( 'NONE',  ( -1.000000000000000000, 0.000000000000000000, 0.000000000000000000 ) ) ;
#6810 = DIRECTION ( 'NONE',  ( -0.000000000000000000, 1.000000000000000000, 0.000000000000000000 ) ) ;
#6811 = ADVANCED_FACE ( 'NONE', ( #18734 ), #7023, .T. ) ;
#6812 = ORIENTED_EDGE ( 'NONE', *, *, #14737, .F. ) ;
#6813 = EDGE_CURVE ( 'NONE', #21676, #14602, #19904, .T. ) ;
#6814 = DIRECTION ( 'NONE',  ( 0.000000000000000000, 0.9945218953682737340, -0.1045284632676505010 ) ) ;
#6815 = CIRCLE ( 'NONE', #19509, 0.02570000000000176310 ) ;
#6816 = CARTESIAN_POINT ( 'NONE',  ( 10.00000000000000000, 17.83210509884670714, -21.83428559348744002 ) ) ;
#6817 = ORIENTED_EDGE ( 'NONE', *, *, #7319, .F. ) ;
#6818 = ADVANCED_FACE ( 'NONE', ( #17296 ), #13756, .T. ) ;
#6819 = EDGE_CURVE ( 'NONE', #5724, #8570, #5447, .T. ) ;
#6820 = DIRECTION ( 'NONE',  ( 1.000000000000000000, 0.000000000000000000, 0.000000000000000000 ) ) ;
#6821 = ORIENTED_EDGE ( 'NONE', *, *, #16994, .F. ) ;
#6822 = AXIS2_PLACEMENT_3D ( 'NONE', #9151, #5312, #15898 ) ;
#6823 = DIRECTION ( 'NONE',  ( -1.000000000000000000, 0.000000000000000000, 0.000000000000000000 ) ) ;
#6824 = VERTEX_POINT ( 'NONE', #8561 ) ;
#6825 = ORIENTED_EDGE ( 'NONE', *, *, #8964, .T. ) ;
#6826 = AXIS2_PLACEMENT_3D ( 'NONE', #7636, #14373, #18029 ) ;
#6827 = ORIENTED_EDGE ( 'NONE', *, *, #21182, .F. ) ;
#6828 = ORIENTED_EDGE ( 'NONE', *, *, #2959, .F. ) ;
#6829 = CARTESIAN_POINT ( 'NONE',  ( 10.00000000000000000, -46.07110168784872428, 74.97635353408365688 ) ) ;
#6830 = ORIENTED_EDGE ( 'NONE', *, *, #19713, .F. ) ;
#6831 = DIRECTION ( 'NONE',  ( -1.000000000000000000, 0.000000000000000000, 0.000000000000000000 ) ) ;
#6832 = CIRCLE ( 'NONE', #21291, 44.99999999999998579 ) ;
#6833 = CARTESIAN_POINT ( 'NONE',  ( 10.00000000000000000, -14.02138820414970688, 83.89630571862279851 ) ) ;
#6834 = DIRECTION ( 'NONE',  ( 1.000000000000000000, 0.000000000000000000, 0.000000000000000000 ) ) ;
#6835 = DIRECTION ( 'NONE',  ( 1.000000000000000000, 0.000000000000000000, 0.000000000000000000 ) ) ;
#6836 = CARTESIAN_POINT ( 'NONE',  ( 10.00000000000000000, -7.409634587002906336, -27.19958299168165183 ) ) ;
#6837 = AXIS2_PLACEMENT_3D ( 'NONE', #19480, #8984, #10644 ) ;
#6838 = AXIS2_PLACEMENT_3D ( 'NONE', #6179, #20976, #11251 ) ;
#6839 = CARTESIAN_POINT ( 'NONE',  ( 10.00000000000000000, 18.31866948046765842, 26.23788002993730117 ) ) ;
#6840 = DIRECTION ( 'NONE',  ( 0.000000000000000000, 0.000000000000000000, 1.000000000000000000 ) ) ;
#6841 = CIRCLE ( 'NONE', #6142, 92.50100000000000477 ) ;
#6842 = CARTESIAN_POINT ( 'NONE',  ( 10.00000000000000000, -25.17124263951018293, 12.69364185792209909 ) ) ;
#6843 = CARTESIAN_POINT ( 'NONE',  ( 0.000000000000000000, 0.000000000000000000, 0.000000000000000000 ) ) ;
#6844 = CARTESIAN_POINT ( 'NONE',  ( 0.000000000000000000, -60.65279801375299229, -63.75921967137679047 ) ) ;
#6845 = VERTEX_POINT ( 'NONE', #17182 ) ;
#6846 = AXIS2_PLACEMENT_3D ( 'NONE', #19295, #17536, #950 ) ;
#6847 = CARTESIAN_POINT ( 'NONE',  ( 0.000000000000000000, -57.53593069156421791, 72.42963261300944566 ) ) ;
#6848 = EDGE_LOOP ( 'NONE', ( #96, #12052 ) ) ;
#6849 = FACE_BOUND ( 'NONE', #8128, .T. ) ;
#6850 = ORIENTED_EDGE ( 'NONE', *, *, #7196, .F. ) ;
#6851 = VECTOR ( 'NONE', #8322, 1000.000000000000000 ) ;
#6852 = ORIENTED_EDGE ( 'NONE', *, *, #4193, .F. ) ;
#6853 = EDGE_LOOP ( 'NONE', ( #14851, #5704, #3270, #11015 ) ) ;
#6854 = DIRECTION ( 'NONE',  ( -1.000000000000000000, -0.000000000000000000, -0.000000000000000000 ) ) ;
#6855 = ORIENTED_EDGE ( 'NONE', *, *, #2840, .T. ) ;
#6856 = CARTESIAN_POINT ( 'NONE',  ( 0.000000000000000000, 0.000000000000000000, 0.000000000000000000 ) ) ;
#6857 = CARTESIAN_POINT ( 'NONE',  ( -8.900000000000012790, 0.000000000000000000, 0.000000000000000000 ) ) ;
#6858 = DIRECTION ( 'NONE',  ( -1.000000000000000000, -0.000000000000000000, 0.000000000000000000 ) ) ;
#6859 = CARTESIAN_POINT ( 'NONE',  ( 10.00000000000000000, 0.000000000000000000, 0.000000000000000000 ) ) ;
#6860 = DIRECTION ( 'NONE',  ( -1.000000000000000000, 0.000000000000000000, 0.000000000000000000 ) ) ;
#6861 = CARTESIAN_POINT ( 'NONE',  ( 10.00000000000000000, -28.15804365424196121, -1.358152127006266197 ) ) ;
#6862 = TOROIDAL_SURFACE ( 'NONE', #3331, 105.0992000000000104, 0.2041999999999998816 ) ;
#6863 = EDGE_CURVE ( 'NONE', #14822, #8942, #15290, .T. ) ;
#6864 = VERTEX_POINT ( 'NONE', #2041 ) ;
#6865 = PRODUCT_DEFINITION_SHAPE ( 'NONE', 'NONE',  #21864 ) ;
#6866 = CIRCLE ( 'NONE', #18500, 44.99999999999999289 ) ;
#6867 = FACE_OUTER_BOUND ( 'NONE', #12716, .T. ) ;
#6868 = ORIENTED_EDGE ( 'NONE', *, *, #17682, .T. ) ;
#6869 = ADVANCED_FACE ( 'NONE', ( #8780 ), #386, .F. ) ;
#6870 = EDGE_LOOP ( 'NONE', ( #925, #5663, #4204, #5952 ) ) ;
#6871 = LINE ( 'NONE', #8739, #13436 ) ;
#6872 = AXIS2_PLACEMENT_3D ( 'NONE', #5204, #11938, #9526 ) ;
#6873 = ORIENTED_EDGE ( 'NONE', *, *, #20358, .F. ) ;
#6874 = CIRCLE ( 'NONE', #19212, 44.99999999999999289 ) ;
#6875 = CYLINDRICAL_SURFACE ( 'NONE', #650, 44.99999999999999289 ) ;
#6876 = ORIENTED_EDGE ( 'NONE', *, *, #12022, .F. ) ;
#6877 = ORIENTED_EDGE ( 'NONE', *, *, #21396, .F. ) ;
#6878 = APPLICATION_PROTOCOL_DEFINITION ( 'draft international standard', 'automotive_design', 1998, #17866 ) ;
#6879 = AXIS2_PLACEMENT_3D ( 'NONE', #3153, #21707, #6592 ) ;
#6880 = FACE_OUTER_BOUND ( 'NONE', #17996, .T. ) ;
#6881 = ORIENTED_EDGE ( 'NONE', *, *, #17706, .T. ) ;
#6882 = VECTOR ( 'NONE', #8201, 1000.000000000000000 ) ;
#6883 = CARTESIAN_POINT ( 'NONE',  ( 10.00000000000000000, 0.000000000000000000, 0.000000000000000000 ) ) ;
#6884 = LINE ( 'NONE', #8431, #18893 ) ;
#6885 = CYLINDRICAL_SURFACE ( 'NONE', #10167, 88.00000000000000000 ) ;
#6886 = CARTESIAN_POINT ( 'NONE',  ( 10.00000000000000000, -18.94217447942616417, 85.93715160505946926 ) ) ;
#6887 = CARTESIAN_POINT ( 'NONE',  ( 0.000000000000000000, 0.000000000000000000, 0.000000000000000000 ) ) ;
#6888 = DIRECTION ( 'NONE',  ( 1.000000000000000000, 0.000000000000000000, 0.000000000000000000 ) ) ;
#6889 = DIRECTION ( 'NONE',  ( 0.000000000000000000, -0.9848077530122096857, 0.1736481776669207000 ) ) ;
#6890 = AXIS2_PLACEMENT_3D ( 'NONE', #868, #4291, #7503 ) ;
#6891 = EDGE_CURVE ( 'NONE', #12476, #12259, #8272, .T. ) ;
#6893 = ADVANCED_FACE ( 'NONE', ( #15850 ), #15944, .F. ) ;
#6892 = CIRCLE ( 'NONE', #6534, 44.99999999999999289 ) ;
#6894 = VERTEX_POINT ( 'NONE', #21153 ) ;
#6895 = AXIS2_PLACEMENT_3D ( 'NONE', #19312, #8921, #4178 ) ;
#6896 = AXIS2_PLACEMENT_3D ( 'NONE', #18158, #1460, #4340 ) ;
#6897 = CIRCLE ( 'NONE', #12876, 88.00000000000000000 ) ;
#6898 = CARTESIAN_POINT ( 'NONE',  ( 10.00000000000000000, -1.959304526717615902, -27.42911093658677402 ) ) ;
#6899 = DIRECTION ( 'NONE',  ( -1.000000000000000000, 0.000000000000000000, 0.000000000000000000 ) ) ;
#6900 = ORIENTED_EDGE ( 'NONE', *, *, #10393, .T. ) ;
#6901 = DIRECTION ( 'NONE',  ( -1.000000000000000000, 0.000000000000000000, 0.000000000000000000 ) ) ;
#6902 = ORIENTED_EDGE ( 'NONE', *, *, #2017, .T. ) ;
#6903 = EDGE_CURVE ( 'NONE', #15915, #10612, #6166, .T. ) ;
#6904 = VERTEX_POINT ( 'NONE', #7551 ) ;
#6905 = DIRECTION ( 'NONE',  ( 1.000000000000000000, 0.000000000000000000, 0.000000000000000000 ) ) ;
#6906 = ORIENTED_EDGE ( 'NONE', *, *, #18781, .T. ) ;
#6907 = AXIS2_PLACEMENT_3D ( 'NONE', #16205, #1068, #20957 ) ;
#6908 = VERTEX_POINT ( 'NONE', #2688 ) ;
#6909 = LINE ( 'NONE', #21702, #16378 ) ;
#6910 = CARTESIAN_POINT ( 'NONE',  ( 0.000000000000000000, -29.29369617358527833, 87.74003855418389719 ) ) ;
#6911 = ORIENTED_EDGE ( 'NONE', *, *, #9054, .T. ) ;
#6912 = AXIS2_PLACEMENT_3D ( 'NONE', #18864, #17419, #9008 ) ;
#6913 = EDGE_CURVE ( 'NONE', #14686, #3581, #1214, .T. ) ;
#6914 = LINE ( 'NONE', #21820, #7576 ) ;
#6915 = CARTESIAN_POINT ( 'NONE',  ( 0.000000000000000000, 24.73395913766463750, 12.01774797440586084 ) ) ;
#6916 = DIRECTION ( 'NONE',  ( 0.000000000000000000, 0.9993908270190958731, -0.03489949670249761771 ) ) ;
#6917 = PLANE ( 'NONE',  #14621 ) ;
#6918 = CARTESIAN_POINT ( 'NONE',  ( 5.000000000000000000, -51.18896083639217665, -71.57995730992236361 ) ) ;
#6919 = FACE_OUTER_BOUND ( 'NONE', #11533, .T. ) ;
#6920 = ADVANCED_FACE ( 'NONE', ( #17721 ), #7348, .F. ) ;
#6921 = EDGE_CURVE ( 'NONE', #1002, #18170, #846, .T. ) ;
#6922 = AXIS2_PLACEMENT_3D ( 'NONE', #9766, #4692, #9882 ) ;
#6923 = ORIENTED_EDGE ( 'NONE', *, *, #18059, .T. ) ;
#6924 = VECTOR ( 'NONE', #15055, 1000.000000000000000 ) ;
#6925 = CARTESIAN_POINT ( 'NONE',  ( 0.000000000000000000, -35.34277389771592226, 85.48288328206373876 ) ) ;
#6926 = ADVANCED_FACE ( 'NONE', ( #17831 ), #5903, .F. ) ;
#6927 = DIRECTION ( 'NONE',  ( 0.000000000000000000, 0.000000000000000000, 1.000000000000000000 ) ) ;
#6928 = ORIENTED_EDGE ( 'NONE', *, *, #21625, .T. ) ;
#6929 = VECTOR ( 'NONE', #20503, 1000.000000000000000 ) ;
#6930 = CIRCLE ( 'NONE', #19978, 88.00000000000000000 ) ;
#6931 = CIRCLE ( 'NONE', #4438, 44.99999999999998579 ) ;
#6932 = CARTESIAN_POINT ( 'NONE',  ( -10.00000000000000000, 0.000000000000000000, 0.000000000000000000 ) ) ;
#6933 = ORIENTED_EDGE ( 'NONE', *, *, #4737, .F. ) ;
#6934 = DIRECTION ( 'NONE',  ( -1.000000000000000000, -0.000000000000000000, 0.000000000000000000 ) ) ;
#6935 = CARTESIAN_POINT ( 'NONE',  ( -10.00000000000000000, 0.000000000000000000, 0.000000000000000000 ) ) ;
#6936 = ORIENTED_EDGE ( 'NONE', *, *, #21606, .F. ) ;
#6937 = EDGE_CURVE ( 'NONE', #12778, #2153, #20613, .T. ) ;
#6938 = ORIENTED_EDGE ( 'NONE', *, *, #13797, .T. ) ;
#6939 = ORIENTED_EDGE ( 'NONE', *, *, #10591, .F. ) ;
#6940 = EDGE_LOOP ( 'NONE', ( #6440, #11152, #15220, #3878 ) ) ;
#6941 = CARTESIAN_POINT ( 'NONE',  ( 10.00000000000000000, 2.481790431839256517, 92.46770094066594936 ) ) ;
#6942 = EDGE_CURVE ( 'NONE', #15480, #11066, #9199, .T. ) ;
#6943 = ORIENTED_EDGE ( 'NONE', *, *, #11129, .F. ) ;
#6944 = DIRECTION ( 'NONE',  ( 0.000000000000000000, 0.9702957262759954737, 0.2419218955996715048 ) ) ;
#6945 = DIRECTION ( 'NONE',  ( -1.000000000000000000, 0.000000000000000000, 0.000000000000000000 ) ) ;
#6946 = CARTESIAN_POINT ( 'NONE',  ( 0.000000000000000000, 26.69209308833507777, 6.612652082459410607 ) ) ;
#6947 = CARTESIAN_POINT ( 'NONE',  ( 7.999999999999979572, 1.393954219129475159E-14, 113.8250000000000171 ) ) ;
#6948 = CARTESIAN_POINT ( 'NONE',  ( 1.500000000000000000, 15.00000000000000000, 7.000000000000000000 ) ) ;
#6949 = CIRCLE ( 'NONE', #19980, 0.02569999999999482421 ) ;
#6950 = EDGE_CURVE ( 'NONE', #7932, #15044, #505, .T. ) ;
#6951 = AXIS2_PLACEMENT_3D ( 'NONE', #13143, #19890, #18249 ) ;
#6952 = CARTESIAN_POINT ( 'NONE',  ( 10.00000000000000000, -84.80486432185169576, -36.94008646920480743 ) ) ;
#6953 = CARTESIAN_POINT ( 'NONE',  ( 0.000000000000000000, 0.000000000000000000, 0.000000000000000000 ) ) ;
#6954 = CARTESIAN_POINT ( 'NONE',  ( 5.000000000000000000, 5.000000000000000000, 15.00000000000000000 ) ) ;
#6955 = DIRECTION ( 'NONE',  ( -1.000000000000000000, 0.000000000000000000, 0.000000000000000000 ) ) ;
#6956 = EDGE_CURVE ( 'NONE', #16874, #10308, #12848, .T. ) ;
#6957 = DIRECTION ( 'NONE',  ( 1.000000000000000000, 0.000000000000000000, 0.000000000000000000 ) ) ;
#6958 = DIRECTION ( 'NONE',  ( 0.000000000000000000, 0.000000000000000000, -1.000000000000000000 ) ) ;
#6959 = ORIENTED_EDGE ( 'NONE', *, *, #6475, .F. ) ;
#6960 = CIRCLE ( 'NONE', #20009, 44.99999999999999289 ) ;
#6961 = ORIENTED_EDGE ( 'NONE', *, *, #7423, .T. ) ;
#6962 = DIRECTION ( 'NONE',  ( -1.000000000000000000, -0.000000000000000000, -0.000000000000000000 ) ) ;
#6963 = AXIS2_PLACEMENT_3D ( 'NONE', #889, #16140, #4310 ) ;
#6964 = ORIENTED_EDGE ( 'NONE', *, *, #1620, .T. ) ;
#6965 = ORIENTED_EDGE ( 'NONE', *, *, #9467, .T. ) ;
#6966 = ORIENTED_EDGE ( 'NONE', *, *, #8548, .T. ) ;
#6967 = FACE_BOUND ( 'NONE', #14250, .T. ) ;
#6968 = EDGE_LOOP ( 'NONE', ( #2823, #18183, #2557, #12321 ) ) ;
#6969 = CARTESIAN_POINT ( 'NONE',  ( 10.00000000000000000, 0.000000000000000000, 0.000000000000000000 ) ) ;
#6970 = CARTESIAN_POINT ( 'NONE',  ( 0.000000000000000000, 76.53853822674039975, -43.42639941457040464 ) ) ;
#6971 = EDGE_CURVE ( 'NONE', #9520, #15915, #21319, .T. ) ;
#6972 = CIRCLE ( 'NONE', #3080, 44.99999999999999289 ) ;
#6973 = CARTESIAN_POINT ( 'NONE',  ( 10.00000000000000000, 84.90234713953992696, -5.175025661882965089 ) ) ;
#6974 = VECTOR ( 'NONE', #17654, 1000.000000000000000 ) ;
#6975 = CARTESIAN_POINT ( 'NONE',  ( 0.000000000000000000, -41.89587599971492438, -77.38692120905515992 ) ) ;
#6976 = DIRECTION ( 'NONE',  ( 0.000000000000000000, 0.2079116908177599254, -0.9781476007338055778 ) ) ;
#6977 = AXIS2_PLACEMENT_3D ( 'NONE', #11146, #4845, #14794 ) ;
#6978 = DIRECTION ( 'NONE',  ( 0.000000000000000000, 0.000000000000000000, 1.000000000000000000 ) ) ;
#6979 = CARTESIAN_POINT ( 'NONE',  ( -8.900000000000018119, 1.456105044186203057E-14, 118.9000000000000199 ) ) ;
#6980 = ORIENTED_EDGE ( 'NONE', *, *, #13637, .T. ) ;
#6981 = FACE_OUTER_BOUND ( 'NONE', #20229, .T. ) ;
#6982 = EDGE_LOOP ( 'NONE', ( #1697, #20377, #18611, #15913 ) ) ;
#6983 = ORIENTED_EDGE ( 'NONE', *, *, #11908, .F. ) ;
#6984 = CIRCLE ( 'NONE', #12622, 45.00000000000000000 ) ;
#6985 = CARTESIAN_POINT ( 'NONE',  ( 10.00000000000000000, 32.56745702629844175, -78.57830605990621109 ) ) ;
#6986 = ORIENTED_EDGE ( 'NONE', *, *, #16829, .F. ) ;
#6987 = VERTEX_POINT ( 'NONE', #7451 ) ;
#6988 = CIRCLE ( 'NONE', #11915, 44.99999999999998579 ) ;
#6989 = CARTESIAN_POINT ( 'NONE',  ( 0.000000000000000000, -83.35585896458606214, -16.94078559808036033 ) ) ;
#6990 = EDGE_LOOP ( 'NONE', ( #11368, #1646, #11315, #8851 ) ) ;
#6991 = DIRECTION ( 'NONE',  ( 0.000000000000000000, 0.000000000000000000, 1.000000000000000000 ) ) ;
#6992 = CYLINDRICAL_SURFACE ( 'NONE', #19601, 92.50100000000000477 ) ;
#6993 = CARTESIAN_POINT ( 'NONE',  ( 7.999999999999979572, 0.000000000000000000, 0.000000000000000000 ) ) ;
#6994 = CARTESIAN_POINT ( 'NONE',  ( 0.000000000000000000, -84.19736439813780748, -38.30455363801015523 ) ) ;
#6995 = EDGE_CURVE ( 'NONE', #20174, #6864, #5796, .T. ) ;
#6996 = DIRECTION ( 'NONE',  ( 0.000000000000000000, 0.000000000000000000, -1.000000000000000000 ) ) ;
#6997 = DIRECTION ( 'NONE',  ( -1.000000000000000000, 0.000000000000000000, -0.000000000000000000 ) ) ;
#6998 = LINE ( 'NONE', #12174, #13327 ) ;
#6999 = AXIS2_PLACEMENT_3D ( 'NONE', #8426, #15153, #27 ) ;
#7000 = VECTOR ( 'NONE', #2472, 1000.000000000000000 ) ;
#7001 = AXIS2_PLACEMENT_3D ( 'NONE', #21803, #9638, #1267 ) ;
#7002 = VECTOR ( 'NONE', #10777, 1000.000000000000000 ) ;
#7003 = ORIENTED_EDGE ( 'NONE', *, *, #9162, .T. ) ;
#7004 = AXIS2_PLACEMENT_3D ( 'NONE', #20688, #13498, #6889 ) ;
#7005 = DIRECTION ( 'NONE',  ( 1.000000000000000000, 0.000000000000000000, 0.000000000000000000 ) ) ;
#7006 = FACE_OUTER_BOUND ( 'NONE', #1885, .T. ) ;
#7007 = ORIENTED_EDGE ( 'NONE', *, *, #4736, .T. ) ;
#7008 = CARTESIAN_POINT ( 'NONE',  ( 10.00000000000000000, 60.65655256511237781, 59.63197188857542841 ) ) ;
#7009 = EDGE_LOOP ( 'NONE', ( #11576, #9675, #6348, #15047 ) ) ;
#7010 = AXIS2_PLACEMENT_3D ( 'NONE', #9703, #21760, #18571 ) ;
#7011 = EDGE_LOOP ( 'NONE', ( #20829, #7621, #16237, #9192 ) ) ;
#7012 = CARTESIAN_POINT ( 'NONE',  ( 0.000000000000000000, 0.000000000000000000, 0.000000000000000000 ) ) ;
#7013 = ORIENTED_EDGE ( 'NONE', *, *, #944, .F. ) ;
#7014 = EDGE_CURVE ( 'NONE', #8843, #3553, #13566, .T. ) ;
#7015 = AXIS2_PLACEMENT_3D ( 'NONE', #787, #14264, #21017 ) ;
#7016 = ORIENTED_EDGE ( 'NONE', *, *, #19736, .F. ) ;
#7017 = CYLINDRICAL_SURFACE ( 'NONE', #12838, 123.0000000000000000 ) ;
#7018 = CARTESIAN_POINT ( 'NONE',  ( 5.000000000000000888, -13.56333590713994575, -28.98337314858449076 ) ) ;
#7019 = AXIS2_PLACEMENT_3D ( 'NONE', #1992, #8733, #17018 ) ;
#7020 = DIRECTION ( 'NONE',  ( -1.000000000000000000, -0.000000000000000000, -0.000000000000000000 ) ) ;
#7021 = CARTESIAN_POINT ( 'NONE',  ( -1.500000000000000000, 0.000000000000000000, 15.00000000000000000 ) ) ;
#7022 = DIRECTION ( 'NONE',  ( 0.000000000000000000, 0.4067366430758009854, -0.9135454576426005335 ) ) ;
#7023 = CYLINDRICAL_SURFACE ( 'NONE', #13905, 7.500000000000020428 ) ;
#7024 = ADVANCED_FACE ( 'NONE', ( #12515 ), #19267, .F. ) ;
#7025 = CARTESIAN_POINT ( 'NONE',  ( 10.00000000000000000, 52.96496548042853192, 66.55750800669373746 ) ) ;
#7026 = FACE_OUTER_BOUND ( 'NONE', #13111, .T. ) ;
#7027 = ORIENTED_EDGE ( 'NONE', *, *, #16988, .T. ) ;
#7028 = DIRECTION ( 'NONE',  ( 0.000000000000000000, 0.000000000000000000, -1.000000000000000000 ) ) ;
#7029 = EDGE_CURVE ( 'NONE', #13846, #16223, #9301, .T. ) ;
#7030 = CIRCLE ( 'NONE', #10526, 44.99999999999999289 ) ;
#7031 = CARTESIAN_POINT ( 'NONE',  ( 10.00000000000000000, -24.73395913766455578, -12.01774797440602427 ) ) ;
#7032 = EDGE_LOOP ( 'NONE', ( #9905, #17663, #19258, #18570 ) ) ;
#7033 = CIRCLE ( 'NONE', #15844, 3.000000000000000444 ) ;
#7034 = CIRCLE ( 'NONE', #1746, 12.00000000000000000 ) ;
#7035 = FACE_OUTER_BOUND ( 'NONE', #5300, .T. ) ;
#7036 = VERTEX_POINT ( 'NONE', #6125 ) ;
#7037 = CARTESIAN_POINT ( 'NONE',  ( 1.129531546211678616, 8.434754829127421589E-16, 6.887500000000022382 ) ) ;
#7038 = CARTESIAN_POINT ( 'NONE',  ( 0.000000000000000000, 21.69483248597422076, 16.89761061231787309 ) ) ;
#7039 = ORIENTED_EDGE ( 'NONE', *, *, #8929, .T. ) ;
#7040 = DIRECTION ( 'NONE',  ( 0.000000000000000000, 0.000000000000000000, 1.000000000000000000 ) ) ;
#7042 = EDGE_CURVE ( 'NONE', #21518, #18065, #21334, .T. ) ;
#7041 = EDGE_LOOP ( 'NONE', ( #12543, #13663, #10360, #11595 ) ) ;
#7043 = EDGE_CURVE ( 'NONE', #21588, #13276, #19209, .T. ) ;
#7044 = ORIENTED_EDGE ( 'NONE', *, *, #2485, .T. ) ;
#7045 = EDGE_CURVE ( 'NONE', #2607, #12265, #3688, .T. ) ;
#7046 = DIRECTION ( 'NONE',  ( -1.000000000000000000, 0.000000000000000000, 0.000000000000000000 ) ) ;
#7047 = ORIENTED_EDGE ( 'NONE', *, *, #2606, .F. ) ;
#7048 = CARTESIAN_POINT ( 'NONE',  ( 5.000000000000002665, 86.54587337002898551, -15.93147207946920396 ) ) ;
#7049 = AXIS2_PLACEMENT_3D ( 'NONE', #19375, #16494, #14832 ) ;
#7050 = EDGE_CURVE ( 'NONE', #5365, #9724, #14617, .T. ) ;
#7051 = DIRECTION ( 'NONE',  ( 0.000000000000000000, 0.000000000000000000, 1.000000000000000000 ) ) ;
#7052 = CARTESIAN_POINT ( 'NONE',  ( -7.440711023145607506, 0.000000000000000000, -115.1000000000000227 ) ) ;
#7053 = CARTESIAN_POINT ( 'NONE',  ( 10.00000000000000000, 9.992993448021948666, -26.36019881529875519 ) ) ;
#7054 = AXIS2_PLACEMENT_3D ( 'NONE', #3273, #11888, #3385 ) ;
#7055 = CIRCLE ( 'NONE', #9487, 92.50100000000000477 ) ;
#7056 = CARTESIAN_POINT ( 'NONE',  ( 7.599999999999998757, 0.000000000000000000, 0.000000000000000000 ) ) ;
#7057 = LINE ( 'NONE', #20425, #234 ) ;
#7058 = CARTESIAN_POINT ( 'NONE',  ( -10.00000000000000000, 0.000000000000000000, 0.000000000000000000 ) ) ;
#7059 = DIRECTION ( 'NONE',  ( 0.000000000000000000, -0.9945218953682742891, 0.1045284632676436315 ) ) ;
#7060 = ORIENTED_EDGE ( 'NONE', *, *, #3381, .F. ) ;
#7061 = LINE ( 'NONE', #15440, #19389 ) ;
#7062 = EDGE_CURVE ( 'NONE', #9931, #20877, #4030, .T. ) ;
#7063 = DIRECTION ( 'NONE',  ( 0.000000000000000000, 0.000000000000000000, 1.000000000000000000 ) ) ;
#7064 = EDGE_CURVE ( 'NONE', #7682, #9443, #4049, .T. ) ;
#7065 = DIRECTION ( 'NONE',  ( -1.000000000000000000, -0.000000000000000000, 0.000000000000000000 ) ) ;
#7066 = ORIENTED_EDGE ( 'NONE', *, *, #7566, .T. ) ;
#7067 = CARTESIAN_POINT ( 'NONE',  ( 1.114299999999999846, 8.409404640385035208E-16, 6.866799999999992465 ) ) ;
#7068 = ORIENTED_EDGE ( 'NONE', *, *, #331, .F. ) ;
#7069 = VECTOR ( 'NONE', #15602, 1000.000000000000000 ) ;
#7070 = CARTESIAN_POINT ( 'NONE',  ( 0.000000000000000000, -18.31866948046748078, -26.23788002993743262 ) ) ;
#7071 = AXIS2_PLACEMENT_3D ( 'NONE', #14872, #21605, #4494 ) ;
#7072 = ADVANCED_FACE ( 'NONE', ( #9744 ), #111, .F. ) ;
#7073 = ORIENTED_EDGE ( 'NONE', *, *, #16128, .T. ) ;
#7074 = ORIENTED_EDGE ( 'NONE', *, *, #12306, .F. ) ;
#7075 = ORIENTED_EDGE ( 'NONE', *, *, #18685, .F. ) ;
#7076 = DIRECTION ( 'NONE',  ( 1.000000000000000000, 0.000000000000000000, 0.000000000000000000 ) ) ;
#7077 = ADVANCED_FACE ( 'NONE', ( #9629 ), #13587, .F. ) ;
#7078 = ORIENTED_EDGE ( 'NONE', *, *, #4782, .T. ) ;
#7079 = CARTESIAN_POINT ( 'NONE',  ( 10.00000000000000000, 15.25521607131237722, -23.70650506194154872 ) ) ;
#7080 = CARTESIAN_POINT ( 'NONE',  ( 5.000000000000000000, -12.46320060045744071, 29.47318494484024853 ) ) ;
#7081 = DIRECTION ( 'NONE',  ( 0.000000000000000000, 1.000000000000000000, -1.224646799147353207E-16 ) ) ;
#7082 = CARTESIAN_POINT ( 'NONE',  ( 10.00000000000000000, 0.000000000000000000, 0.000000000000000000 ) ) ;
#7083 = DIRECTION ( 'NONE',  ( 1.000000000000000000, 0.000000000000000000, 0.000000000000000000 ) ) ;
#7084 = DIRECTION ( 'NONE',  ( -1.000000000000000000, 0.000000000000000000, 0.000000000000000000 ) ) ;
#7085 = VECTOR ( 'NONE', #16262, 1000.000000000000000 ) ;
#7086 = DIRECTION ( 'NONE',  ( 1.000000000000000000, -0.000000000000000000, -0.000000000000000000 ) ) ;
#7087 = CARTESIAN_POINT ( 'NONE',  ( 10.00000000000000000, 69.74988376404090218, -53.65588238863266213 ) ) ;
#7088 = EDGE_CURVE ( 'NONE', #5100, #2139, #5465, .T. ) ;
#7089 = EDGE_LOOP ( 'NONE', ( #21493, #4362, #11442, #5278 ) ) ;
#7090 = ADVANCED_FACE ( 'NONE', ( #19705 ), #2807, .T. ) ;
#7091 = DIRECTION ( 'NONE',  ( 0.000000000000000000, 0.9510565162951523099, 0.3090169943749512260 ) ) ;
#7092 = EDGE_LOOP ( 'NONE', ( #6486, #11924, #18399, #19334 ) ) ;
#7093 = EDGE_CURVE ( 'NONE', #11653, #17995, #18527, .T. ) ;
#7094 = EDGE_CURVE ( 'NONE', #13650, #20538, #16275, .T. ) ;
#7095 = ORIENTED_EDGE ( 'NONE', *, *, #3235, .F. ) ;
#7096 = CARTESIAN_POINT ( 'NONE',  ( 10.00000000000000000, -84.79630770241078608, -6.691460262316255125 ) ) ;
#7097 = EDGE_LOOP ( 'NONE', ( #10339, #8073, #3917, #17088 ) ) ;
#7098 = AXIS2_PLACEMENT_3D ( 'NONE', #18908, #353, #451 ) ;
#7099 = VERTEX_POINT ( 'NONE', #12843 ) ;
#7100 = LINE ( 'NONE', #17362, #14052 ) ;
#7101 = VERTEX_POINT ( 'NONE', #7884 ) ;
#7102 = CARTESIAN_POINT ( 'NONE',  ( 10.00000000000000000, 0.000000000000000000, 0.000000000000000000 ) ) ;
#7103 = CARTESIAN_POINT ( 'NONE',  ( 10.00000000000000000, 25.17124263951009411, 12.69364185792227495 ) ) ;
#7104 = FACE_OUTER_BOUND ( 'NONE', #15204, .T. ) ;
#7105 = CARTESIAN_POINT ( 'NONE',  ( 10.00000000000000000, -62.44821182181044605, -68.23969402963567177 ) ) ;
#7106 = DIRECTION ( 'NONE',  ( 0.000000000000000000, 0.000000000000000000, -1.000000000000000000 ) ) ;
#7107 = DIRECTION ( 'NONE',  ( 0.000000000000000000, 0.000000000000000000, -1.000000000000000000 ) ) ;
#7108 = DIRECTION ( 'NONE',  ( 1.000000000000000000, 0.000000000000000000, 0.000000000000000000 ) ) ;
#7109 = PRESENTATION_LAYER_ASSIGNMENT (  '', '', ( #6414 ) ) ;
#7110 = ORIENTED_EDGE ( 'NONE', *, *, #17293, .T. ) ;
#7111 = DIRECTION ( 'NONE',  ( -1.000000000000000000, 0.000000000000000000, -0.000000000000000000 ) ) ;
#7112 = CARTESIAN_POINT ( 'NONE',  ( 0.000000000000000000, -83.48638250753248258, 27.82128566055087049 ) ) ;
#7113 = ORIENTED_EDGE ( 'NONE', *, *, #13345, .T. ) ;
#7114 = CARTESIAN_POINT ( 'NONE',  ( 10.00000000000000888, 4.000000000000000000, 1.000000000000000000 ) ) ;
#7115 = ORIENTED_EDGE ( 'NONE', *, *, #13249, .T. ) ;
#7116 = DIRECTION ( 'NONE',  ( 0.000000000000000000, 0.000000000000000000, 1.000000000000000000 ) ) ;
#7117 = ORIENTED_EDGE ( 'NONE', *, *, #15442, .T. ) ;
#7118 = VERTEX_POINT ( 'NONE', #8613 ) ;
#7119 = LINE ( 'NONE', #12400, #21678 ) ;
#7120 = DIRECTION ( 'NONE',  ( 0.000000000000000000, -0.9848077530122062440, -0.1736481776669404620 ) ) ;
#7121 = DIRECTION ( 'NONE',  ( 0.000000000000000000, 0.000000000000000000, -1.000000000000000000 ) ) ;
#7122 = LINE ( 'NONE', #13852, #20051 ) ;
#7123 = DIRECTION ( 'NONE',  ( 1.000000000000000000, 0.000000000000000000, 0.000000000000000000 ) ) ;
#7124 = DIRECTION ( 'NONE',  ( 1.000000000000000000, -0.000000000000000000, -0.000000000000000000 ) ) ;
#7125 = CARTESIAN_POINT ( 'NONE',  ( 10.00000000000000000, -75.45728100697627383, 39.26051685139039193 ) ) ;
#7126 = DIRECTION ( 'NONE',  ( 0.000000000000000000, 0.000000000000000000, -1.000000000000000000 ) ) ;
#7127 = ORIENTED_EDGE ( 'NONE', *, *, #9012, .T. ) ;
#7128 = DIRECTION ( 'NONE',  ( -1.000000000000000000, 0.000000000000000000, -0.000000000000000000 ) ) ;
#7129 = ADVANCED_FACE ( 'NONE', ( #19595 ), #1141, .F. ) ;
#7130 = VERTEX_POINT ( 'NONE', #16384 ) ;
#7131 = DIRECTION ( 'NONE',  ( 0.000000000000000000, 0.000000000000000000, 1.000000000000000000 ) ) ;
#7132 = ORIENTED_EDGE ( 'NONE', *, *, #13274, .F. ) ;
#7133 = CARTESIAN_POINT ( 'NONE',  ( 10.00000000000000000, 17.70753755129066320, -21.03896658273954046 ) ) ;
#7134 = CARTESIAN_POINT ( 'NONE',  ( 10.00000000000000000, 14.53731623274961571, -23.34226719384889748 ) ) ;
#7135 = VERTEX_POINT ( 'NONE', #1255 ) ;
#7136 = EDGE_CURVE ( 'NONE', #2434, #9160, #7938, .T. ) ;
#7137 = ORIENTED_EDGE ( 'NONE', *, *, #9915, .T. ) ;
#7138 = ORIENTED_EDGE ( 'NONE', *, *, #1470, .F. ) ;
#7139 = ORIENTED_EDGE ( 'NONE', *, *, #14360, .F. ) ;
#7140 = FACE_OUTER_BOUND ( 'NONE', #2791, .T. ) ;
#7141 = ORIENTED_EDGE ( 'NONE', *, *, #1792, .T. ) ;
#7142 = CARTESIAN_POINT ( 'NONE',  ( 5.000000000000000000, -23.37352460145268651, -21.85585385440903750 ) ) ;
#7143 = CYLINDRICAL_SURFACE ( 'NONE', #11793, 92.50100000000000477 ) ;
#7144 = DIRECTION ( 'NONE',  ( -1.000000000000000000, -0.000000000000000000, -0.000000000000000000 ) ) ;
#7145 = DIRECTION ( 'NONE',  ( -1.000000000000000000, 0.000000000000000000, -0.000000000000000000 ) ) ;
#7146 = CARTESIAN_POINT ( 'NONE',  ( 10.00000000000000000, 51.10509369859540385, -77.10190917907144126 ) ) ;
#7147 = LINE ( 'NONE', #5606, #12571 ) ;
#7148 = CIRCLE ( 'NONE', #20199, 88.00000000000000000 ) ;
#7149 = CARTESIAN_POINT ( 'NONE',  ( 0.000000000000000000, 31.75612719289740937, 3.943144139962659445 ) ) ;
#7150 = VERTEX_POINT ( 'NONE', #19811 ) ;
#7151 = DIRECTION ( 'NONE',  ( -0.000000000000000000, -0.000000000000000000, -1.000000000000000000 ) ) ;
#7152 = VECTOR ( 'NONE', #7291, 1000.000000000000000 ) ;
#7153 = DIRECTION ( 'NONE',  ( 1.000000000000000000, 0.000000000000000000, 0.000000000000000000 ) ) ;
#7154 = EDGE_CURVE ( 'NONE', #15205, #9318, #11410, .T. ) ;
#7155 = EDGE_CURVE ( 'NONE', #16266, #10715, #16498, .T. ) ;
#7156 = ADVANCED_FACE ( 'NONE', ( #8108 ), #10164, .F. ) ;
#7157 = CIRCLE ( 'NONE', #3619, 88.00000000000000000 ) ;
#7158 = CARTESIAN_POINT ( 'NONE',  ( 10.00000000000000000, 29.29369617358583255, -87.74003855418371245 ) ) ;
#7159 = ORIENTED_EDGE ( 'NONE', *, *, #14086, .F. ) ;
#7160 = EDGE_CURVE ( 'NONE', #12492, #19254, #5117, .T. ) ;
#7161 = CYLINDRICAL_SURFACE ( 'NONE', #20095, 45.00000000000000000 ) ;
#7162 = VERTEX_POINT ( 'NONE', #20769 ) ;
#7163 = DIRECTION ( 'NONE',  ( -1.000000000000000000, 0.000000000000000000, 0.000000000000000000 ) ) ;
#7164 = VERTEX_POINT ( 'NONE', #439 ) ;
#7165 = ORIENTED_EDGE ( 'NONE', *, *, #5967, .T. ) ;
#7166 = ORIENTED_EDGE ( 'NONE', *, *, #3634, .F. ) ;
#7167 = EDGE_CURVE ( 'NONE', #17904, #19570, #7567, .T. ) ;
#7168 = DIRECTION ( 'NONE',  ( 0.000000000000000000, 0.000000000000000000, 1.000000000000000000 ) ) ;
#7169 = VECTOR ( 'NONE', #6858, 1000.000000000000000 ) ;
#7170 = TOROIDAL_SURFACE ( 'NONE', #6838, 118.9000000000000199, 1.100000000000015854 ) ;
#7171 = CARTESIAN_POINT ( 'NONE',  ( 5.000000000000002665, -12.90135963484022241, -87.04915231966658951 ) ) ;
#7172 = CARTESIAN_POINT ( 'NONE',  ( 10.00000000000000000, 64.66851233300727131, 55.25552418572984692 ) ) ;
#7173 = DIRECTION ( 'NONE',  ( -1.000000000000000000, 0.000000000000000000, 0.000000000000000000 ) ) ;
#7174 = VECTOR ( 'NONE', #5563, 1000.000000000000000 ) ;
#7175 = PRODUCT_DEFINITION_CONTEXT ( 'detailed design', #5318, 'design' ) ;
#7176 = ADVANCED_FACE ( 'NONE', ( #1990 ), #18896, .F. ) ;
#7177 = CARTESIAN_POINT ( 'NONE',  ( 0.000000000000000000, 27.26034713664097353, -7.182859710736244629 ) ) ;
#7178 = DIRECTION ( 'NONE',  ( 0.000000000000000000, 0.000000000000000000, -1.000000000000000000 ) ) ;
#7179 = DIRECTION ( 'NONE',  ( 0.000000000000000000, 0.000000000000000000, 1.000000000000000000 ) ) ;
#7180 = DIRECTION ( 'NONE',  ( 1.000000000000000000, 0.000000000000000000, 0.000000000000000000 ) ) ;
#7181 = DIRECTION ( 'NONE',  ( 1.000000000000000000, 0.000000000000000000, 0.000000000000000000 ) ) ;
#7182 =( GEOMETRIC_REPRESENTATION_CONTEXT ( 3 ) GLOBAL_UNCERTAINTY_ASSIGNED_CONTEXT ( ( #18078 ) ) GLOBAL_UNIT_ASSIGNED_CONTEXT ( ( #18440, #10019, #8164 ) ) REPRESENTATION_CONTEXT ( 'NONE', 'WORKASPACE' ) );
#7183 = ADVANCED_FACE ( 'NONE', ( #13811 ), #17242, .F. ) ;
#7184 = EDGE_LOOP ( 'NONE', ( #19721, #15620, #6633, #18465 ) ) ;
#7185 = CYLINDRICAL_SURFACE ( 'NONE', #8698, 32.00000000000000000 ) ;
#7186 = AXIS2_PLACEMENT_3D ( 'NONE', #4188, #18076, #4699 ) ;
#7187 = ORIENTED_EDGE ( 'NONE', *, *, #2457, .F. ) ;
#7188 = EDGE_CURVE ( 'NONE', #11274, #19400, #10746, .T. ) ;
#7189 = ORIENTED_EDGE ( 'NONE', *, *, #19225, .T. ) ;
#7190 = CIRCLE ( 'NONE', #19532, 27.49900000000000233 ) ;
#7191 = ORIENTED_EDGE ( 'NONE', *, *, #4332, .F. ) ;
#7192 = DIRECTION ( 'NONE',  ( -1.000000000000000000, 0.000000000000000000, 0.000000000000000000 ) ) ;
#7193 = CIRCLE ( 'NONE', #123, 11.99999999999999822 ) ;
#7194 = VERTEX_POINT ( 'NONE', #5522 ) ;
#7195 = ORIENTED_EDGE ( 'NONE', *, *, #20951, .T. ) ;
#7196 = EDGE_CURVE ( 'NONE', #8891, #3730, #3344, .T. ) ;
#7197 = DIRECTION ( 'NONE',  ( 1.000000000000000000, -0.000000000000000000, -0.000000000000000000 ) ) ;
#7198 = CIRCLE ( 'NONE', #13549, 27.49900000000000233 ) ;
#7199 = ORIENTED_EDGE ( 'NONE', *, *, #18702, .T. ) ;
#7200 = ADVANCED_FACE ( 'NONE', ( #12043 ), #4081, .F. ) ;
#7201 = DIRECTION ( 'NONE',  ( 1.000000000000000000, 0.000000000000000000, 0.000000000000000000 ) ) ;
#7202 = CYLINDRICAL_SURFACE ( 'NONE', #8551, 44.99999999999998579 ) ;
#7203 = CIRCLE ( 'NONE', #13177, 32.00000000000000000 ) ;
#7204 = DIRECTION ( 'NONE',  ( -1.000000000000000000, -0.000000000000000000, 0.000000000000000000 ) ) ;
#7205 = CARTESIAN_POINT ( 'NONE',  ( -7.600000000000001421, 1.287093988729475069E-14, 105.0992000000000104 ) ) ;
#7206 = LINE ( 'NONE', #3777, #10800 ) ;
#7207 = EDGE_CURVE ( 'NONE', #1843, #13321, #1231, .T. ) ;
#7208 = AXIS2_PLACEMENT_3D ( 'NONE', #13750, #9980, #11660 ) ;
#7209 = EDGE_CURVE ( 'NONE', #12422, #1308, #16746, .T. ) ;
#7210 = DIRECTION ( 'NONE',  ( 0.000000000000000000, -6.982962677686266711E-15, 1.000000000000000000 ) ) ;
#7211 = DIRECTION ( 'NONE',  ( 0.000000000000000000, 0.000000000000000000, 1.000000000000000000 ) ) ;
#7212 = DIRECTION ( 'NONE',  ( -1.000000000000000000, 0.000000000000000000, -0.000000000000000000 ) ) ;
#7213 = VERTEX_POINT ( 'NONE', #344 ) ;
#7214 = AXIS2_PLACEMENT_3D ( 'NONE', #10104, #16850, #1719 ) ;
#7215 = EDGE_CURVE ( 'NONE', #16161, #4858, #8731, .T. ) ;
#7216 = DIRECTION ( 'NONE',  ( 0.000000000000000000, -0.5877852522924632561, -0.8090169943749546677 ) ) ;
#7217 = AXIS2_PLACEMENT_3D ( 'NONE', #20519, #6945, #18541 ) ;
#7218 = CARTESIAN_POINT ( 'NONE',  ( 10.00000000000000000, -83.03980459022491800, 18.42770452393216374 ) ) ;
#7219 = EDGE_LOOP ( 'NONE', ( #13290, #14269, #20218, #3954 ) ) ;
#7220 = DIRECTION ( 'NONE',  ( 0.000000000000000000, 0.000000000000000000, 1.000000000000000000 ) ) ;
#7221 = ORIENTED_EDGE ( 'NONE', *, *, #14476, .F. ) ;
#7222 = VECTOR ( 'NONE', #4237, 1000.000000000000000 ) ;
#7223 = CARTESIAN_POINT ( 'NONE',  ( 0.000000000000000000, 0.000000000000000000, 0.000000000000000000 ) ) ;
#7224 = VERTEX_POINT ( 'NONE', #7403 ) ;
#7225 = ORIENTED_EDGE ( 'NONE', *, *, #21793, .T. ) ;
#7226 = DIRECTION ( 'NONE',  ( -1.000000000000000000, -0.000000000000000000, -0.000000000000000000 ) ) ;
#7227 = DIRECTION ( 'NONE',  ( 0.000000000000000000, 0.000000000000000000, 1.000000000000000000 ) ) ;
#7228 = VECTOR ( 'NONE', #17565, 1000.000000000000000 ) ;
#7229 = CARTESIAN_POINT ( 'NONE',  ( -10.00000000000000000, 0.000000000000000000, 0.000000000000000000 ) ) ;
#7230 = DIRECTION ( 'NONE',  ( -1.000000000000000000, -0.000000000000000000, -0.000000000000000000 ) ) ;
#7231 = AXIS2_PLACEMENT_3D ( 'NONE', #8170, #14899, #20101 ) ;
#7232 = CYLINDRICAL_SURFACE ( 'NONE', #9016, 88.00000000000000000 ) ;
#7233 = DIRECTION ( 'NONE',  ( 1.000000000000000000, 0.000000000000000000, 0.000000000000000000 ) ) ;
#7234 = AXIS2_PLACEMENT_3D ( 'NONE', #19977, #10018, #1636 ) ;
#7235 = EDGE_CURVE ( 'NONE', #9876, #13595, #5416, .T. ) ;
#7236 = CARTESIAN_POINT ( 'NONE',  ( 10.00000000000000000, 2.208823992044147033, 85.03123271466937183 ) ) ;
#7237 = LINE ( 'NONE', #5361, #8176 ) ;
#7239 = CIRCLE ( 'NONE', #19574, 44.99999999999998579 ) ;
#7238 = AXIS2_PLACEMENT_3D ( 'NONE', #487, #12199, #13965 ) ;
#7240 = ORIENTED_EDGE ( 'NONE', *, *, #5534, .F. ) ;
#7241 = VECTOR ( 'NONE', #19422, 1000.000000000000000 ) ;
#7242 = DIRECTION ( 'NONE',  ( 1.000000000000000000, -0.000000000000000000, 0.000000000000000000 ) ) ;
#7243 = ORIENTED_EDGE ( 'NONE', *, *, #4508, .F. ) ;
#7244 = CARTESIAN_POINT ( 'NONE',  ( 0.000000000000000000, 84.90234713953985590, 5.175025661884123274 ) ) ;
#7245 = ORIENTED_EDGE ( 'NONE', *, *, #8371, .T. ) ;
#7246 = DIRECTION ( 'NONE',  ( -1.000000000000000000, 0.000000000000000000, -0.000000000000000000 ) ) ;
#7247 = CIRCLE ( 'NONE', #19591, 44.99999999999999289 ) ;
#7248 = VECTOR ( 'NONE', #5937, 1000.000000000000000 ) ;
#7249 = CYLINDRICAL_SURFACE ( 'NONE', #9852, 5.000000000000000888 ) ;
#7250 = AXIS2_PLACEMENT_3D ( 'NONE', #3467, #20809, #2556 ) ;
#7251 = ORIENTED_EDGE ( 'NONE', *, *, #19746, .F. ) ;
#7252 = CIRCLE ( 'NONE', #19596, 92.50100000000000477 ) ;
#7253 = SURFACE_SIDE_STYLE ('',( #20728 ) ) ;
#7254 = AXIS2_PLACEMENT_3D ( 'NONE', #12485, #13936, #680 ) ;
#7255 = ORIENTED_EDGE ( 'NONE', *, *, #15632, .F. ) ;
#7256 = ORIENTED_EDGE ( 'NONE', *, *, #19273, .T. ) ;
#7257 = ORIENTED_EDGE ( 'NONE', *, *, #8200, .F. ) ;
#7258 = LINE ( 'NONE', #8893, #21303 ) ;
#7259 = EDGE_LOOP ( 'NONE', ( #10898, #6227, #3781, #14499 ) ) ;
#7260 = LINE ( 'NONE', #7373, #147 ) ;
#7261 = DIRECTION ( 'NONE',  ( 0.000000000000000000, 0.000000000000000000, 1.000000000000000000 ) ) ;
#7262 = ADVANCED_FACE ( 'NONE', ( #13704 ), #18786, .T. ) ;
#7263 = CARTESIAN_POINT ( 'NONE',  ( 0.000000000000000000, -92.49798535263882115, -0.7467976319030308341 ) ) ;
#7264 = CARTESIAN_POINT ( 'NONE',  ( 0.000000000000000000, -32.56745702629687855, -78.57830605990686479 ) ) ;
#7265 = DIRECTION ( 'NONE',  ( -1.000000000000000000, -0.000000000000000000, -0.000000000000000000 ) ) ;
#7266 = AXIS2_PLACEMENT_3D ( 'NONE', #5261, #18522, #12493 ) ;
#7267 = DIRECTION ( 'NONE',  ( 0.000000000000000000, 0.000000000000000000, 1.000000000000000000 ) ) ;
#7268 = VECTOR ( 'NONE', #7890, 1000.000000000000000 ) ;
#7269 = ORIENTED_EDGE ( 'NONE', *, *, #2343, .F. ) ;
#7270 = EDGE_CURVE ( 'NONE', #8974, #4047, #1922, .T. ) ;
#7271 = CIRCLE ( 'NONE', #5853, 88.00000000000000000 ) ;
#7272 = CARTESIAN_POINT ( 'NONE',  ( 10.00000000000000000, -61.60362715319078575, 62.84101464466223774 ) ) ;
#7273 = AXIS2_PLACEMENT_3D ( 'NONE', #5729, #2514, #3856 ) ;
#7274 = CARTESIAN_POINT ( 'NONE',  ( 1.199999999999992628, 0.000000000000000000, 0.000000000000000000 ) ) ;
#7275 = CARTESIAN_POINT ( 'NONE',  ( 10.00000000000000000, 89.12061559554365431, -24.77803214283454736 ) ) ;
#7276 = ORIENTED_EDGE ( 'NONE', *, *, #9486, .F. ) ;
#7277 = CARTESIAN_POINT ( 'NONE',  ( 0.000000000000000000, -64.95266917914358373, 59.37298010462950515 ) ) ;
#7278 = ORIENTED_EDGE ( 'NONE', *, *, #16211, .T. ) ;
#7279 = DIRECTION ( 'NONE',  ( 0.000000000000000000, 0.000000000000000000, 1.000000000000000000 ) ) ;
#7280 = VERTEX_POINT ( 'NONE', #3865 ) ;
#7281 = APPLICATION_CONTEXT ( 'automotive_design' ) ;
#7282 = ORIENTED_EDGE ( 'NONE', *, *, #19302, .T. ) ;
#7283 = AXIS2_PLACEMENT_3D ( 'NONE', #1556, #3105, #16923 ) ;
#7284 = ORIENTED_EDGE ( 'NONE', *, *, #21055, .F. ) ;
#7285 = CARTESIAN_POINT ( 'NONE',  ( 10.00000000000000000, 0.000000000000000000, 0.000000000000000000 ) ) ;
#7286 = CIRCLE ( 'NONE', #21397, 6.500000000000000000 ) ;
#7287 = ORIENTED_EDGE ( 'NONE', *, *, #473, .F. ) ;
#7288 = AXIS2_PLACEMENT_3D ( 'NONE', #83, #16657, #15211 ) ;
#7289 = FACE_OUTER_BOUND ( 'NONE', #3151, .T. ) ;
#7290 = CARTESIAN_POINT ( 'NONE',  ( 7.500000000000000000, 9.184850993605147944E-16, -3.000000000000000000 ) ) ;
#7291 = DIRECTION ( 'NONE',  ( -1.000000000000000000, 0.000000000000000000, 0.000000000000000000 ) ) ;
#7292 = ADVANCED_FACE ( 'NONE', ( #14021 ), #20553, .F. ) ;
#7293 = FACE_OUTER_BOUND ( 'NONE', #11482, .T. ) ;
#7294 = CARTESIAN_POINT ( 'NONE',  ( 10.00000000000000000, 37.96946988134172329, 76.11510229470873412 ) ) ;
#7295 = CARTESIAN_POINT ( 'NONE',  ( -10.00000000000000000, 0.000000000000000000, 0.000000000000000000 ) ) ;
#7296 = FACE_OUTER_BOUND ( 'NONE', #11098, .T. ) ;
#7297 = CARTESIAN_POINT ( 'NONE',  ( 5.000000000000000000, 86.77540292929701593, 14.62974526292747868 ) ) ;
#7298 = AXIS2_PLACEMENT_3D ( 'NONE', #15217, #2967, #18230 ) ;
#7299 = ORIENTED_EDGE ( 'NONE', *, *, #10707, .F. ) ;
#7300 = AXIS2_PLACEMENT_3D ( 'NONE', #3100, #6096, #17918 ) ;
#7301 = LINE ( 'NONE', #3644, #17518 ) ;
#7302 = EDGE_CURVE ( 'NONE', #21336, #13824, #10600, .T. ) ;
#7303 = ORIENTED_EDGE ( 'NONE', *, *, #5716, .F. ) ;
#7304 = ORIENTED_EDGE ( 'NONE', *, *, #16785, .F. ) ;
#7305 = ORIENTED_EDGE ( 'NONE', *, *, #14080, .F. ) ;
#7306 = EDGE_CURVE ( 'NONE', #4889, #8180, #10041, .T. ) ;
#7307 = DIRECTION ( 'NONE',  ( -1.000000000000000000, -0.000000000000000000, -0.000000000000000000 ) ) ;
#7308 = ORIENTED_EDGE ( 'NONE', *, *, #7707, .T. ) ;
#7309 = ORIENTED_EDGE ( 'NONE', *, *, #2100, .F. ) ;
#7310 = CARTESIAN_POINT ( 'NONE',  ( 0.000000000000000000, 1.959304526717801975, 27.42911093658675981 ) ) ;
#7311 = CIRCLE ( 'NONE', #19657, 44.99999999999999289 ) ;
#7312 = EDGE_CURVE ( 'NONE', #8212, #18019, #12510, .T. ) ;
#7313 = ORIENTED_EDGE ( 'NONE', *, *, #14205, .F. ) ;
#7314 = EDGE_CURVE ( 'NONE', #11159, #2487, #10404, .T. ) ;
#7315 = EDGE_CURVE ( 'NONE', #7892, #13441, #13227, .T. ) ;
#7316 = CARTESIAN_POINT ( 'NONE',  ( 10.00000000000000000, 0.000000000000000000, 0.000000000000000000 ) ) ;
#7317 = CIRCLE ( 'NONE', #20012, 88.00000000000000000 ) ;
#7318 = DIRECTION ( 'NONE',  ( -1.000000000000000000, -0.000000000000000000, -0.000000000000000000 ) ) ;
#7319 = EDGE_CURVE ( 'NONE', #12668, #18181, #20993, .T. ) ;
#7320 = LINE ( 'NONE', #775, #1237 ) ;
#7321 = DIRECTION ( 'NONE',  ( -1.000000000000000000, -0.000000000000000000, -0.000000000000000000 ) ) ;
#7322 = DIRECTION ( 'NONE',  ( -1.000000000000000000, -0.000000000000000000, 0.000000000000000000 ) ) ;
#7323 = LINE ( 'NONE', #21121, #21722 ) ;
#7324 = CARTESIAN_POINT ( 'NONE',  ( -90.00000000000000000, 0.000000000000000000, 0.000000000000000000 ) ) ;
#7325 = DIRECTION ( 'NONE',  ( 0.000000000000000000, 0.000000000000000000, 1.000000000000000000 ) ) ;
#7326 = ORIENTED_EDGE ( 'NONE', *, *, #5449, .T. ) ;
#7327 = EDGE_CURVE ( 'NONE', #8870, #20207, #14278, .T. ) ;
#7328 = CIRCLE ( 'NONE', #11913, 88.00000000000000000 ) ;
#7329 = AXIS2_PLACEMENT_3D ( 'NONE', #19277, #9209, #16179 ) ;
#7330 = CYLINDRICAL_SURFACE ( 'NONE', #10517, 44.99999999999998579 ) ;
#7331 = EDGE_CURVE ( 'NONE', #791, #17102, #4764, .T. ) ;
#7332 = AXIS2_PLACEMENT_3D ( 'NONE', #9657, #1065, #7803 ) ;
#7333 = DIRECTION ( 'NONE',  ( 1.000000000000000000, 0.000000000000000000, 0.000000000000000000 ) ) ;
#7334 = EDGE_LOOP ( 'NONE', ( #13793, #15353, #357, #15176 ) ) ;
#7335 = CARTESIAN_POINT ( 'NONE',  ( 5.000000000000000000, 57.06999622551805373, 66.98518889142101784 ) ) ;
#7336 = ORIENTED_EDGE ( 'NONE', *, *, #5005, .T. ) ;
#7337 = EDGE_CURVE ( 'NONE', #15117, #2159, #17119, .T. ) ;
#7338 = DIRECTION ( 'NONE',  ( -1.000000000000000000, -0.000000000000000000, -0.000000000000000000 ) ) ;
#7339 = EDGE_LOOP ( 'NONE', ( #4586, #4273 ) ) ;
#7340 = ORIENTED_EDGE ( 'NONE', *, *, #11805, .T. ) ;
#7341 = CARTESIAN_POINT ( 'NONE',  ( 10.00000000000000000, 46.89573839703275127, 79.73220629831503459 ) ) ;
#7342 = EDGE_CURVE ( 'NONE', #5623, #11894, #20983, .T. ) ;
#7343 = DIRECTION ( 'NONE',  ( -1.000000000000000000, -0.000000000000000000, -0.000000000000000000 ) ) ;
#7344 = DIRECTION ( 'NONE',  ( 0.000000000000000000, -6.938893903907230744E-15, 1.000000000000000000 ) ) ;
#7345 = AXIS2_PLACEMENT_3D ( 'NONE', #17275, #11746, #20693 ) ;
#7346 = DIRECTION ( 'NONE',  ( 0.000000000000000000, 0.000000000000000000, 1.000000000000000000 ) ) ;
#7347 = CIRCLE ( 'NONE', #5231, 88.00000000000000000 ) ;
#7348 = CYLINDRICAL_SURFACE ( 'NONE', #8965, 88.00000000000000000 ) ;
#7349 = AXIS2_PLACEMENT_3D ( 'NONE', #18717, #15265, #5444 ) ;
#7350 = CARTESIAN_POINT ( 'NONE',  ( 0.000000000000000000, 27.40684453873966575, 16.51862198942017557 ) ) ;
#7351 = CARTESIAN_POINT ( 'NONE',  ( -10.00000000000000000, 0.000000000000000000, 0.000000000000000000 ) ) ;
#7352 = VERTEX_POINT ( 'NONE', #16115 ) ;
#7353 = DIRECTION ( 'NONE',  ( 0.000000000000000000, -0.8290375725550350738, -0.5591929034707566748 ) ) ;
#7354 = ORIENTED_EDGE ( 'NONE', *, *, #8157, .T. ) ;
#7355 = EDGE_CURVE ( 'NONE', #9424, #6845, #7589, .T. ) ;
#7356 = FACE_OUTER_BOUND ( 'NONE', #3356, .T. ) ;
#7357 = ORIENTED_EDGE ( 'NONE', *, *, #7952, .T. ) ;
#7358 = CIRCLE ( 'NONE', #11944, 44.99999999999999289 ) ;
#7359 = CARTESIAN_POINT ( 'NONE',  ( 0.000000000000000000, 75.87763420127893710, -44.57111876559645225 ) ) ;
#7360 = AXIS2_PLACEMENT_3D ( 'NONE', #3527, #11393, #20210 ) ;
#7361 = AXIS2_PLACEMENT_3D ( 'NONE', #8421, #3445, #10064 ) ;
#7362 = CARTESIAN_POINT ( 'NONE',  ( 0.000000000000000000, -7.409634587002906336, -27.19958299168165183 ) ) ;
#7363 = AXIS2_PLACEMENT_3D ( 'NONE', #3103, #14817, #4761 ) ;
#7364 = VERTEX_POINT ( 'NONE', #11257 ) ;
#7365 = EDGE_CURVE ( 'NONE', #8963, #13997, #10923, .T. ) ;
#7366 = FILL_AREA_STYLE ('',( #823 ) ) ;
#7367 = ORIENTED_EDGE ( 'NONE', *, *, #2882, .T. ) ;
#7368 = ORIENTED_EDGE ( 'NONE', *, *, #8004, .F. ) ;
#7369 = EDGE_LOOP ( 'NONE', ( #10759, #15540, #18537, #4319 ) ) ;
#7370 = DIRECTION ( 'NONE',  ( 1.000000000000000000, 0.000000000000000000, 0.000000000000000000 ) ) ;
#7371 = DIRECTION ( 'NONE',  ( 1.000000000000000000, 0.000000000000000000, 0.000000000000000000 ) ) ;
#7372 = ORIENTED_EDGE ( 'NONE', *, *, #13338, .F. ) ;
#7373 = CARTESIAN_POINT ( 'NONE',  ( 10.00000000000000000, 28.15804365424197186, 10.64184787299392454 ) ) ;
#7374 = CARTESIAN_POINT ( 'NONE',  ( -140.0000508000000536, 2.828427124746190291, -1.000000000000000000 ) ) ;
#7375 = DIRECTION ( 'NONE',  ( 1.000000000000000000, -0.000000000000000000, -0.000000000000000000 ) ) ;
#7376 = CARTESIAN_POINT ( 'NONE',  ( 10.00000000000000000, -92.32475887865429343, 5.707354816230212791 ) ) ;
#7377 = FACE_OUTER_BOUND ( 'NONE', #13302, .T. ) ;
#7378 = CIRCLE ( 'NONE', #15121, 44.99999999999999289 ) ;
#7379 = CIRCLE ( 'NONE', #12659, 92.50099999999999056 ) ;
#7380 = PRESENTATION_LAYER_ASSIGNMENT (  '', '', ( #21830 ) ) ;
#7381 = ORIENTED_EDGE ( 'NONE', *, *, #2755, .F. ) ;
#7382 = CIRCLE ( 'NONE', #4918, 12.00000000000000000 ) ;
#7383 = CARTESIAN_POINT ( 'NONE',  ( 0.000000000000000000, -33.95793648385871677, 86.04239391577978324 ) ) ;
#7384 = CYLINDRICAL_SURFACE ( 'NONE', #16769, 88.00000000000000000 ) ;
#7385 = DIRECTION ( 'NONE',  ( 0.000000000000000000, 0.000000000000000000, 1.000000000000000000 ) ) ;
#7386 = ORIENTED_EDGE ( 'NONE', *, *, #162, .T. ) ;
#7387 = CARTESIAN_POINT ( 'NONE',  ( 5.000000000000000000, 24.89070495400736505, 84.40647372620510680 ) ) ;
#7388 = EDGE_LOOP ( 'NONE', ( #18469, #606 ) ) ;
#7389 = LINE ( 'NONE', #15660, #8768 ) ;
#7390 = ORIENTED_EDGE ( 'NONE', *, *, #19282, .F. ) ;
#7391 = CIRCLE ( 'NONE', #7049, 44.99999999999999289 ) ;
#7392 = ORIENTED_EDGE ( 'NONE', *, *, #18412, .T. ) ;
#7393 = ORIENTED_EDGE ( 'NONE', *, *, #17705, .T. ) ;
#7394 = AXIS2_PLACEMENT_3D ( 'NONE', #9902, #17307, #12528 ) ;
#7395 = CARTESIAN_POINT ( 'NONE',  ( 10.00000000000000000, -48.19312842678519360, 70.09002648625178722 ) ) ;
#7396 = ORIENTED_EDGE ( 'NONE', *, *, #6656, .T. ) ;
#7397 = CARTESIAN_POINT ( 'NONE',  ( 0.000000000000000000, 0.000000000000000000, 0.000000000000000000 ) ) ;
#7398 = CARTESIAN_POINT ( 'NONE',  ( -90.00000000000000000, 0.000000000000000000, 0.000000000000000000 ) ) ;
#7399 = CARTESIAN_POINT ( 'NONE',  ( 10.00000000000000000, -10.41137886060169038, 91.91321010181843576 ) ) ;
#7400 = DIRECTION ( 'NONE',  ( -1.000000000000000000, 0.000000000000000000, 0.000000000000000000 ) ) ;
#7401 = DIRECTION ( 'NONE',  ( 0.000000000000000000, 0.000000000000000000, -1.000000000000000000 ) ) ;
#7402 = DIRECTION ( 'NONE',  ( 1.000000000000000000, 0.000000000000000000, 0.000000000000000000 ) ) ;
#7403 = CARTESIAN_POINT ( 'NONE',  ( 0.000000000000000000, -56.05743251323904985, 67.83483072893783117 ) ) ;
#7404 = CARTESIAN_POINT ( 'NONE',  ( 0.000000000000000000, 35.34277389771533961, 85.48288328206398035 ) ) ;
#7405 = FACE_OUTER_BOUND ( 'NONE', #882, .T. ) ;
#7406 = AXIS2_PLACEMENT_3D ( 'NONE', #21149, #18157, #2682 ) ;
#7407 = CIRCLE ( 'NONE', #7768, 92.50099999999999056 ) ;
#7408 = ORIENTED_EDGE ( 'NONE', *, *, #4563, .T. ) ;
#7409 = DIRECTION ( 'NONE',  ( -1.000000000000000000, 0.000000000000000000, 0.000000000000000000 ) ) ;
#7410 = ORIENTED_EDGE ( 'NONE', *, *, #7828, .F. ) ;
#7411 = EDGE_CURVE ( 'NONE', #16782, #7213, #16045, .T. ) ;
#7412 = ORIENTED_EDGE ( 'NONE', *, *, #14599, .T. ) ;
#7413 = ORIENTED_EDGE ( 'NONE', *, *, #4894, .T. ) ;
#7414 = EDGE_LOOP ( 'NONE', ( #14475, #6335, #16176, #14312 ) ) ;
#7415 = ORIENTED_EDGE ( 'NONE', *, *, #4865, .F. ) ;
#7416 = EDGE_CURVE ( 'NONE', #8339, #20733, #9684, .T. ) ;
#7417 = VERTEX_POINT ( 'NONE', #2859 ) ;
#7418 = DIRECTION ( 'NONE',  ( 0.000000000000000000, -1.000000000000000000, 0.000000000000000000 ) ) ;
#7419 = ORIENTED_EDGE ( 'NONE', *, *, #8672, .T. ) ;
#7420 = CIRCLE ( 'NONE', #17314, 88.00000000000000000 ) ;
#7421 = CARTESIAN_POINT ( 'NONE',  ( 10.00000000000000000, -9.366510754379408610, 25.85466064925422458 ) ) ;
#7422 = DIRECTION ( 'NONE',  ( 0.000000000000000000, 0.06975647374411846069, 0.9975640502598246417 ) ) ;
#7423 = EDGE_CURVE ( 'NONE', #11372, #16515, #8641, .T. ) ;
#7424 = DIRECTION ( 'NONE',  ( 1.000000000000000000, 0.000000000000000000, 0.000000000000000000 ) ) ;
#7425 = DIRECTION ( 'NONE',  ( 0.000000000000000000, -0.4694715627858975782, 0.8829475928589234357 ) ) ;
#7426 = CARTESIAN_POINT ( 'NONE',  ( 0.000000000000000000, -0.6609040254617754018, 87.99751818016873983 ) ) ;
#7427 = DIRECTION ( 'NONE',  ( 0.000000000000000000, 1.000000000000000000, -1.224646799147353207E-16 ) ) ;
#7428 = CARTESIAN_POINT ( 'NONE',  ( 0.000000000000000000, -83.89484365856893078, -26.56417150043033359 ) ) ;
#7429 = CARTESIAN_POINT ( 'NONE',  ( 0.000000000000000000, 0.000000000000000000, 0.000000000000000000 ) ) ;
#7430 = ORIENTED_EDGE ( 'NONE', *, *, #8165, .T. ) ;
#7431 = DIRECTION ( 'NONE',  ( -1.000000000000000000, -0.000000000000000000, 0.000000000000000000 ) ) ;
#7432 = EDGE_CURVE ( 'NONE', #783, #10259, #12332, .T. ) ;
#7433 = ADVANCED_FACE ( 'NONE', ( #11147 ), #17896, .T. ) ;
#7434 = VECTOR ( 'NONE', #18325, 1000.000000000000000 ) ;
#7435 = CARTESIAN_POINT ( 'NONE',  ( 6.123233995736766282E-16, -5.000000000000000000, 5.000000000000004441 ) ) ;
#7436 = EDGE_CURVE ( 'NONE', #14422, #4009, #18799, .T. ) ;
#7437 = DIRECTION ( 'NONE',  ( 0.000000000000000000, 0.6427876096865405842, -0.7660444431189771253 ) ) ;
#7438 = ORIENTED_EDGE ( 'NONE', *, *, #4588, .F. ) ;
#7439 = DIRECTION ( 'NONE',  ( 0.000000000000000000, 0.000000000000000000, -1.000000000000000000 ) ) ;
#7440 = ORIENTED_EDGE ( 'NONE', *, *, #17361, .F. ) ;
#7441 = SHAPE_REPRESENTATION_RELATIONSHIP ( 'NONE' , 'NONE' ,  #6003, #6437 ) ;
#7442 = CARTESIAN_POINT ( 'NONE',  ( 0.000000000000000000, 0.000000000000000000, 0.000000000000000000 ) ) ;
#7443 = EDGE_LOOP ( 'NONE', ( #20837, #20609, #11786, #3346 ) ) ;
#7444 = ORIENTED_EDGE ( 'NONE', *, *, #19727, .F. ) ;
#7445 = DIRECTION ( 'NONE',  ( -1.000000000000000000, -0.000000000000000000, -0.000000000000000000 ) ) ;
#7446 = EDGE_CURVE ( 'NONE', #9701, #16531, #19502, .T. ) ;
#7447 = DIRECTION ( 'NONE',  ( 1.000000000000000000, -0.000000000000000000, -0.000000000000000000 ) ) ;
#7448 = LINE ( 'NONE', #4130, #21106 ) ;
#7449 = DIRECTION ( 'NONE',  ( 0.000000000000000000, 0.8290375725550390706, 0.5591929034707506796 ) ) ;
#7450 = CIRCLE ( 'NONE', #18053, 44.99999999999998579 ) ;
#7451 = CARTESIAN_POINT ( 'NONE',  ( 10.00000000000000000, 12.90135963484081216, 87.04915231966650424 ) ) ;
#7452 = DIRECTION ( 'NONE',  ( 0.000000000000000000, -0.2079116908177467415, -0.9781476007338083534 ) ) ;
#7453 = ADVANCED_FACE ( 'NONE', ( #7615 ), #7940, .F. ) ;
#7454 = CYLINDRICAL_SURFACE ( 'NONE', #17567, 11.99999999999999822 ) ;
#7455 = DIRECTION ( 'NONE',  ( -1.000000000000000000, 0.000000000000000000, 0.000000000000000000 ) ) ;
#7456 = VERTEX_POINT ( 'NONE', #14350 ) ;
#7457 = CARTESIAN_POINT ( 'NONE',  ( 10.00000000000000000, -57.47876254627184522, 62.70072803846370135 ) ) ;
#7458 = ORIENTED_EDGE ( 'NONE', *, *, #6546, .F. ) ;
#7459 = CARTESIAN_POINT ( 'NONE',  ( -1.129531546211723025, 0.000000000000000000, 0.000000000000000000 ) ) ;
#7460 = ORIENTED_EDGE ( 'NONE', *, *, #11908, .T. ) ;
#7461 = EDGE_CURVE ( 'NONE', #1066, #7352, #19136, .T. ) ;
#7462 = DIRECTION ( 'NONE',  ( 1.000000000000000000, 0.000000000000000000, 0.000000000000000000 ) ) ;
#7463 = DIRECTION ( 'NONE',  ( -1.000000000000000000, -0.000000000000000000, -0.000000000000000000 ) ) ;
#7464 = EDGE_LOOP ( 'NONE', ( #999, #17377, #2030, #8451 ) ) ;
#7465 = ORIENTED_EDGE ( 'NONE', *, *, #20383, .F. ) ;
#7466 = VERTEX_POINT ( 'NONE', #18105 ) ;
#7467 = ORIENTED_EDGE ( 'NONE', *, *, #11386, .T. ) ;
#7468 = CARTESIAN_POINT ( 'NONE',  ( 10.00000000000000000, 84.12297548659721258, -12.59025161327029529 ) ) ;
#7469 = DIRECTION ( 'NONE',  ( -1.000000000000000000, 0.000000000000000000, 0.000000000000000000 ) ) ;
#7470 = ORIENTED_EDGE ( 'NONE', *, *, #17724, .F. ) ;
#7471 = EDGE_CURVE ( 'NONE', #1435, #3525, #2962, .T. ) ;
#7472 = FACE_OUTER_BOUND ( 'NONE', #3649, .T. ) ;
#7473 = CARTESIAN_POINT ( 'NONE',  ( 7.599999999999998757, 0.000000000000000000, 0.000000000000000000 ) ) ;
#7474 = DIRECTION ( 'NONE',  ( 1.000000000000000000, 0.000000000000000000, 0.000000000000000000 ) ) ;
#7475 = EDGE_CURVE ( 'NONE', #5601, #5584, #91, .T. ) ;
#7476 = CARTESIAN_POINT ( 'NONE',  ( 10.00000000000000000, 51.18896083639367589, -71.57995730992126937 ) ) ;
#7477 = CARTESIAN_POINT ( 'NONE',  ( 5.000000000000000888, -30.61448696004458725, 9.314139153634121371 ) ) ;
#7478 = VECTOR ( 'NONE', #2074, 1000.000000000000000 ) ;
#7479 = ADVANCED_FACE ( 'NONE', ( #1314 ), #14198, .T. ) ;
#7480 = ORIENTED_EDGE ( 'NONE', *, *, #3565, .T. ) ;
#7481 = EDGE_CURVE ( 'NONE', #8355, #1096, #10319, .T. ) ;
#7482 = CARTESIAN_POINT ( 'NONE',  ( 10.00000000000000000, 51.10509369859433804, 77.10190917907216601 ) ) ;
#7483 = DIRECTION ( 'NONE',  ( 1.000000000000000000, 0.000000000000000000, 0.000000000000000000 ) ) ;
#7484 = DIRECTION ( 'NONE',  ( -1.000000000000000000, -0.000000000000000000, 0.000000000000000000 ) ) ;
#7485 = AXIS2_PLACEMENT_3D ( 'NONE', #16142, #12490, #11170 ) ;
#7486 = EDGE_LOOP ( 'NONE', ( #3623, #5748, #20445, #4635 ) ) ;
#7487 = LINE ( 'NONE', #20962, #17615 ) ;
#7488 = ORIENTED_EDGE ( 'NONE', *, *, #1771, .F. ) ;
#7489 = DIRECTION ( 'NONE',  ( 0.000000000000000000, 0.000000000000000000, 1.000000000000000000 ) ) ;
#7490 = VERTEX_POINT ( 'NONE', #16447 ) ;
#7491 = ORIENTED_EDGE ( 'NONE', *, *, #7549, .T. ) ;
#7492 = ORIENTED_EDGE ( 'NONE', *, *, #7988, .F. ) ;
#7493 = DIRECTION ( 'NONE',  ( -1.000000000000000000, -0.000000000000000000, 0.000000000000000000 ) ) ;
#7494 = ORIENTED_EDGE ( 'NONE', *, *, #21076, .F. ) ;
#7495 = CARTESIAN_POINT ( 'NONE',  ( 10.00000000000000000, -78.01214607583727911, -33.90124636420193838 ) ) ;
#7496 = AXIS2_PLACEMENT_3D ( 'NONE', #7102, #13935, #15484 ) ;
#7497 = DIRECTION ( 'NONE',  ( 0.000000000000000000, 0.000000000000000000, -1.000000000000000000 ) ) ;
#7498 = DIRECTION ( 'NONE',  ( 0.000000000000000000, 0.000000000000000000, 1.000000000000000000 ) ) ;
#7499 = FACE_OUTER_BOUND ( 'NONE', #4359, .T. ) ;
#7500 = CIRCLE ( 'NONE', #10314, 44.99999999999999289 ) ;
#7501 = LINE ( 'NONE', #20868, #16325 ) ;
#7502 = DIRECTION ( 'NONE',  ( -1.000000000000000000, 0.000000000000000000, 0.000000000000000000 ) ) ;
#7503 = DIRECTION ( 'NONE',  ( 0.000000000000000000, 0.000000000000000000, -1.000000000000000000 ) ) ;
#7504 = VECTOR ( 'NONE', #4846, 1000.000000000000000 ) ;
#7505 = LINE ( 'NONE', #17781, #9783 ) ;
#7506 = CARTESIAN_POINT ( 'NONE',  ( 0.000000000000000000, 19.83954325428658194, 82.71385593638699163 ) ) ;
#7507 = FACE_OUTER_BOUND ( 'NONE', #10213, .T. ) ;
#7508 = VERTEX_POINT ( 'NONE', #8490 ) ;
#7509 = VECTOR ( 'NONE', #4868, 1000.000000000000000 ) ;
#7510 = ORIENTED_EDGE ( 'NONE', *, *, #1428, .F. ) ;
#7511 = ORIENTED_EDGE ( 'NONE', *, *, #20997, .T. ) ;
#7512 = AXIS2_PLACEMENT_3D ( 'NONE', #6973, #13702, #20451 ) ;
#7513 = VERTEX_POINT ( 'NONE', #8269 ) ;
#7514 = AXIS2_PLACEMENT_3D ( 'NONE', #7223, #15391, #12504 ) ;
#7515 = EDGE_LOOP ( 'NONE', ( #14154, #561, #3415, #12028 ) ) ;
#7516 = DIRECTION ( 'NONE',  ( -1.000000000000000000, 0.000000000000000000, 0.000000000000000000 ) ) ;
#7517 = VERTEX_POINT ( 'NONE', #1750 ) ;
#7518 = DIRECTION ( 'NONE',  ( 0.000000000000000000, 0.000000000000000000, 1.000000000000000000 ) ) ;
#7519 = CARTESIAN_POINT ( 'NONE',  ( 10.00000000000000000, -92.22057093985034726, 7.197311757040196767 ) ) ;
#7520 = CIRCLE ( 'NONE', #6485, 92.50099999999999056 ) ;
#7521 = DIRECTION ( 'NONE',  ( 1.000000000000000000, 0.000000000000000000, 0.000000000000000000 ) ) ;
#7522 = FACE_OUTER_BOUND ( 'NONE', #8219, .T. ) ;
#7523 = ADVANCED_FACE ( 'NONE', ( #14795 ), #5065, .F. ) ;
#7524 = DIRECTION ( 'NONE',  ( 0.000000000000000000, -0.2756373558170062132, 0.9612616959383166737 ) ) ;
#7525 = DIRECTION ( 'NONE',  ( -1.000000000000000000, 0.000000000000000000, 0.000000000000000000 ) ) ;
#7526 = DIRECTION ( 'NONE',  ( 0.000000000000000000, 0.000000000000000000, 1.000000000000000000 ) ) ;
#7527 = DIRECTION ( 'NONE',  ( -1.000000000000000000, -0.000000000000000000, -0.000000000000000000 ) ) ;
#7528 = ORIENTED_EDGE ( 'NONE', *, *, #2710, .T. ) ;
#7529 = EDGE_CURVE ( 'NONE', #11066, #21052, #7157, .T. ) ;
#7530 = CIRCLE ( 'NONE', #2941, 100.0000000000000284 ) ;
#7531 = DIRECTION ( 'NONE',  ( -1.000000000000000000, 0.000000000000000000, 0.000000000000000000 ) ) ;
#7532 = LINE ( 'NONE', #21134, #11599 ) ;
#7533 = CARTESIAN_POINT ( 'NONE',  ( 10.00000000000000000, -57.47876254627099257, -62.70072803846446163 ) ) ;
#7534 = CIRCLE ( 'NONE', #17783, 88.00000000000000000 ) ;
#7535 = ORIENTED_EDGE ( 'NONE', *, *, #2190, .F. ) ;
#7536 = DIRECTION ( 'NONE',  ( 0.000000000000000000, 0.8290375725550428454, -0.5591929034707450175 ) ) ;
#7537 = EDGE_LOOP ( 'NONE', ( #18748, #21165 ) ) ;
#7538 = APPLICATION_PROTOCOL_DEFINITION ( 'draft international standard', 'automotive_design', 1998, #774 ) ;
#7539 = AXIS2_PLACEMENT_3D ( 'NONE', #21363, #19812, #2906 ) ;
#7540 = CARTESIAN_POINT ( 'NONE',  ( 0.000000000000000000, 69.74988376404020585, 53.65588238863360715 ) ) ;
#7541 = ORIENTED_EDGE ( 'NONE', *, *, #11673, .F. ) ;
#7542 = VERTEX_POINT ( 'NONE', #16662 ) ;
#7543 = CARTESIAN_POINT ( 'NONE',  ( 1.500000000000001332, 0.000000000000000000, 0.000000000000000000 ) ) ;
#7544 = CIRCLE ( 'NONE', #11425, 44.99999999999999289 ) ;
#7545 = FACE_OUTER_BOUND ( 'NONE', #19541, .T. ) ;
#7546 = CARTESIAN_POINT ( 'NONE',  ( 10.00000000000000000, -87.44637528609653998, -9.855528870799524555 ) ) ;
#7547 = DIRECTION ( 'NONE',  ( 1.000000000000000000, -0.000000000000000000, -0.000000000000000000 ) ) ;
#7548 = EDGE_CURVE ( 'NONE', #10938, #8963, #8213, .T. ) ;
#7549 = EDGE_CURVE ( 'NONE', #5771, #9061, #15617, .T. ) ;
#7550 = FACE_OUTER_BOUND ( 'NONE', #17437, .T. ) ;
#7551 = CARTESIAN_POINT ( 'NONE',  ( 10.00000000000000000, 74.39348546125125949, -54.97312363261338675 ) ) ;
#7552 = CYLINDRICAL_SURFACE ( 'NONE', #7894, 126.5000000000000000 ) ;
#7553 = DIRECTION ( 'NONE',  ( 0.000000000000000000, 0.000000000000000000, 1.000000000000000000 ) ) ;
#7554 = CARTESIAN_POINT ( 'NONE',  ( 10.00000000000000000, -72.53479564998751528, -44.42851404693431761 ) ) ;
#7555 = AXIS2_PLACEMENT_3D ( 'NONE', #4243, #804, #21035 ) ;
#7556 = ORIENTED_EDGE ( 'NONE', *, *, #13083, .F. ) ;
#7557 = CARTESIAN_POINT ( 'NONE',  ( 10.00000000000000000, 0.000000000000000000, 0.000000000000000000 ) ) ;
#7558 = CIRCLE ( 'NONE', #11440, 120.0000000000000284 ) ;
#7559 = VERTEX_POINT ( 'NONE', #13121 ) ;
#7560 = AXIS2_PLACEMENT_3D ( 'NONE', #11299, #18048, #9620 ) ;
#7561 = DIRECTION ( 'NONE',  ( 1.000000000000000000, 0.000000000000000000, 0.000000000000000000 ) ) ;
#7562 = ADVANCED_FACE ( 'NONE', ( #15002 ), #9803, .F. ) ;
#7563 = VERTEX_POINT ( 'NONE', #6739 ) ;
#7564 = CARTESIAN_POINT ( 'NONE',  ( 5.000000000000002665, -87.58454185039444440, 8.540961822681374827 ) ) ;
#7565 = EDGE_LOOP ( 'NONE', ( #20513, #21567, #18849, #3474 ) ) ;
#7566 = EDGE_CURVE ( 'NONE', #11073, #19781, #13486, .T. ) ;
#7567 = CIRCLE ( 'NONE', #20293, 88.00000000000000000 ) ;
#7568 = VERTEX_POINT ( 'NONE', #1427 ) ;
#7569 = VERTEX_POINT ( 'NONE', #11910 ) ;
#7570 = CIRCLE ( 'NONE', #14981, 44.99999999999999289 ) ;
#7571 = ORIENTED_EDGE ( 'NONE', *, *, #2167, .F. ) ;
#7573 = AXIS2_PLACEMENT_3D ( 'NONE', #5549, #467, #18716 ) ;
#7572 = CARTESIAN_POINT ( 'NONE',  ( -140.0000508000000536, 2.828427124746190291, 1.000000000000000000 ) ) ;
#7574 = LINE ( 'NONE', #19176, #15455 ) ;
#7575 = ORIENTED_EDGE ( 'NONE', *, *, #2444, .T. ) ;
#7576 = VECTOR ( 'NONE', #3367, 1000.000000000000000 ) ;
#7577 = EDGE_CURVE ( 'NONE', #8085, #2294, #8167, .T. ) ;
#7578 = DIRECTION ( 'NONE',  ( -1.000000000000000000, -0.000000000000000000, -0.000000000000000000 ) ) ;
#7579 = DIRECTION ( 'NONE',  ( -1.000000000000000000, -0.000000000000000000, -0.000000000000000000 ) ) ;
#7580 = EDGE_CURVE ( 'NONE', #3657, #21386, #18661, .T. ) ;
#7581 = CARTESIAN_POINT ( 'NONE',  ( 0.000000000000000000, -78.04699792498179534, 49.64978465107262906 ) ) ;
#7582 = EDGE_CURVE ( 'NONE', #2434, #10630, #19850, .T. ) ;
#7583 = DIRECTION ( 'NONE',  ( 1.000000000000000000, 0.000000000000000000, 0.000000000000000000 ) ) ;
#7584 = CIRCLE ( 'NONE', #14270, 44.99999999999999289 ) ;
#7585 = DIRECTION ( 'NONE',  ( 0.000000000000000000, 0.000000000000000000, -1.000000000000000000 ) ) ;
#7586 = EDGE_CURVE ( 'NONE', #8720, #13591, #18340, .T. ) ;
#7587 = ORIENTED_EDGE ( 'NONE', *, *, #19188, .F. ) ;
#7588 = DIRECTION ( 'NONE',  ( 0.000000000000000000, 0.000000000000000000, 1.000000000000000000 ) ) ;
#7589 = CIRCLE ( 'NONE', #19934, 92.50100000000000477 ) ;
#7590 = CARTESIAN_POINT ( 'NONE',  ( 10.00000000000000000, 21.65267340503250537, 89.93106657554442052 ) ) ;
#7591 = AXIS2_PLACEMENT_3D ( 'NONE', #212, #6957, #16093 ) ;
#7592 = CIRCLE ( 'NONE', #2996, 44.99999999999998579 ) ;
#7593 = LINE ( 'NONE', #11126, #6974 ) ;
#7594 = EDGE_CURVE ( 'NONE', #21723, #14855, #6808, .T. ) ;
#7595 = AXIS2_PLACEMENT_3D ( 'NONE', #7995, #19917, #14725 ) ;
#7596 = ORIENTED_EDGE ( 'NONE', *, *, #12871, .F. ) ;
#7597 = ORIENTED_EDGE ( 'NONE', *, *, #18368, .F. ) ;
#7598 = CARTESIAN_POINT ( 'NONE',  ( 0.000000000000000000, 0.000000000000000000, 0.000000000000000000 ) ) ;
#7599 = EDGE_CURVE ( 'NONE', #15453, #20112, #13856, .T. ) ;
#7600 = CIRCLE ( 'NONE', #885, 45.00000000000000000 ) ;
#7601 = EDGE_LOOP ( 'NONE', ( #9426, #8599, #10144, #2373 ) ) ;
#7602 = EDGE_LOOP ( 'NONE', ( #6748, #16834, #16013, #10563 ) ) ;
#7603 = VERTEX_POINT ( 'NONE', #1641 ) ;
#7604 = CARTESIAN_POINT ( 'NONE',  ( 10.00000000000000000, -25.48117629651196125, 10.33947075754252332 ) ) ;
#7605 = EDGE_CURVE ( 'NONE', #8443, #1388, #21855, .T. ) ;
#7606 = EDGE_LOOP ( 'NONE', ( #1804, #11449, #4530, #19163 ) ) ;
#7607 = CARTESIAN_POINT ( 'NONE',  ( -1.399999999999999911, 6.245698675651501825E-16, 5.100000000000000533 ) ) ;
#7608 = DIRECTION ( 'NONE',  ( -1.000000000000000000, -0.000000000000000000, 0.000000000000000000 ) ) ;
#7609 = DIRECTION ( 'NONE',  ( -1.000000000000000000, -0.000000000000000000, -0.000000000000000000 ) ) ;
#7610 = AXIS2_PLACEMENT_3D ( 'NONE', #1467, #14731, #3231 ) ;
#7611 = CIRCLE ( 'NONE', #15359, 12.00000000000000000 ) ;
#7612 = DIRECTION ( 'NONE',  ( 0.000000000000000000, 0.000000000000000000, 1.000000000000000000 ) ) ;
#7613 = EDGE_CURVE ( 'NONE', #1120, #19953, #518, .T. ) ;
#7614 = DIRECTION ( 'NONE',  ( -0.000000000000000000, -1.000000000000000000, -0.000000000000000000 ) ) ;
#7615 = FACE_OUTER_BOUND ( 'NONE', #13261, .T. ) ;
#7616 = CYLINDRICAL_SURFACE ( 'NONE', #15441, 44.99999999999998579 ) ;
#7617 = DIRECTION ( 'NONE',  ( -1.000000000000000000, 0.000000000000000000, 0.000000000000000000 ) ) ;
#7618 = FACE_OUTER_BOUND ( 'NONE', #17906, .T. ) ;
#7619 = ORIENTED_EDGE ( 'NONE', *, *, #12209, .T. ) ;
#7620 = CIRCLE ( 'NONE', #20331, 45.00000000000000000 ) ;
#7621 = ORIENTED_EDGE ( 'NONE', *, *, #12260, .F. ) ;
#7622 = AXIS2_PLACEMENT_3D ( 'NONE', #20786, #15916, #7518 ) ;
#7623 = ADVANCED_FACE ( 'NONE', ( #412 ), #20741, .F. ) ;
#7624 = AXIS2_PLACEMENT_3D ( 'NONE', #9098, #15849, #708 ) ;
#7625 = ORIENTED_EDGE ( 'NONE', *, *, #21606, .T. ) ;
#7626 = AXIS2_PLACEMENT_3D ( 'NONE', #8961, #466, #14257 ) ;
#7627 = ORIENTED_EDGE ( 'NONE', *, *, #17178, .T. ) ;
#7628 = EDGE_CURVE ( 'NONE', #17995, #15667, #11744, .T. ) ;
#7629 = ORIENTED_EDGE ( 'NONE', *, *, #15542, .T. ) ;
#7630 = CARTESIAN_POINT ( 'NONE',  ( 1.200000000000006617, 6.873330160214519262E-16, 5.612499999999999822 ) ) ;
#7631 = ORIENTED_EDGE ( 'NONE', *, *, #18765, .T. ) ;
#7632 = CARTESIAN_POINT ( 'NONE',  ( 10.00000000000000000, -81.32027326007839463, -44.08455690949136851 ) ) ;
#7633 = CARTESIAN_POINT ( 'NONE',  ( 10.00000000000000000, 35.18804927320529430, 80.65854690202691302 ) ) ;
#7634 = DIRECTION ( 'NONE',  ( 1.000000000000000000, 0.000000000000000000, 0.000000000000000000 ) ) ;
#7635 = DIRECTION ( 'NONE',  ( 1.000000000000000000, 0.000000000000000000, 0.000000000000000000 ) ) ;
#7636 = CARTESIAN_POINT ( 'NONE',  ( 0.000000000000000000, 0.000000000000000000, 25.00000000000000000 ) ) ;
#7637 = CIRCLE ( 'NONE', #13975, 88.00000000000000000 ) ;
#7638 = CARTESIAN_POINT ( 'NONE',  ( 0.000000000000000000, 30.71797041605808687, 82.46457599186561538 ) ) ;
#7639 = AXIS2_PLACEMENT_3D ( 'NONE', #14255, #14149, #17482 ) ;
#7640 = DIRECTION ( 'NONE',  ( -0.000000000000000000, -0.000000000000000000, -1.000000000000000000 ) ) ;
#7641 = DIRECTION ( 'NONE',  ( 1.000000000000000000, 0.000000000000000000, 0.000000000000000000 ) ) ;
#7642 = CARTESIAN_POINT ( 'NONE',  ( 10.00000000000000000, 0.000000000000000000, 0.000000000000000000 ) ) ;
#7643 = ORIENTED_EDGE ( 'NONE', *, *, #13682, .F. ) ;
#7644 = DIRECTION ( 'NONE',  ( 0.000000000000000000, 0.000000000000000000, 1.000000000000000000 ) ) ;
#7645 = EDGE_CURVE ( 'NONE', #659, #1075, #5743, .T. ) ;
#7646 = CARTESIAN_POINT ( 'NONE',  ( 10.00000000000000000, 0.000000000000000000, 0.000000000000000000 ) ) ;
#7647 = CIRCLE ( 'NONE', #20003, 45.00000000000000000 ) ;
#7648 = CYLINDRICAL_SURFACE ( 'NONE', #19770, 88.00000000000000000 ) ;
#7649 = VECTOR ( 'NONE', #11434, 1000.000000000000000 ) ;
#7650 = EDGE_LOOP ( 'NONE', ( #7856, #566, #7195, #9460 ) ) ;
#7651 = CIRCLE ( 'NONE', #3756, 92.50100000000000477 ) ;
#7652 = DIRECTION ( 'NONE',  ( -1.000000000000000000, 0.000000000000000000, 0.000000000000000000 ) ) ;
#7653 = ORIENTED_EDGE ( 'NONE', *, *, #584, .T. ) ;
#7654 = ORIENTED_EDGE ( 'NONE', *, *, #10199, .F. ) ;
#7655 = CIRCLE ( 'NONE', #3787, 92.50100000000000477 ) ;
#7656 = DIRECTION ( 'NONE',  ( 0.000000000000000000, -1.000000000000000000, 0.000000000000000000 ) ) ;
#7657 = LINE ( 'NONE', #2677, #1882 ) ;
#7658 = ORIENTED_EDGE ( 'NONE', *, *, #15237, .F. ) ;
#7659 = ORIENTED_EDGE ( 'NONE', *, *, #14870, .F. ) ;
#7660 = CARTESIAN_POINT ( 'NONE',  ( 10.00000000000000000, -48.19312842678519360, 70.09002648625178722 ) ) ;
#7661 = DIRECTION ( 'NONE',  ( 0.000000000000000000, 0.000000000000000000, 1.000000000000000000 ) ) ;
#7662 = CARTESIAN_POINT ( 'NONE',  ( 5.000000000000000888, 0.6021240089805670603, -31.99433460282943997 ) ) ;
#7663 = DIRECTION ( 'NONE',  ( -1.000000000000000000, 0.000000000000000000, 0.000000000000000000 ) ) ;
#7664 = FACE_OUTER_BOUND ( 'NONE', #10851, .T. ) ;
#7665 = CARTESIAN_POINT ( 'NONE',  ( -10.00000000000000000, 0.000000000000000000, 0.000000000000000000 ) ) ;
#7666 = CARTESIAN_POINT ( 'NONE',  ( 0.000000000000000000, 22.77465461094694632, -15.41136296218063428 ) ) ;
#7667 = DIRECTION ( 'NONE',  ( -1.000000000000000000, -0.000000000000000000, 0.000000000000000000 ) ) ;
#7668 = CYLINDRICAL_SURFACE ( 'NONE', #4504, 44.99999999999999289 ) ;
#7669 = TOROIDAL_SURFACE ( 'NONE', #9415, 6.866799999999992465, 0.02569999999999482421 ) ;
#7670 = EDGE_LOOP ( 'NONE', ( #11705, #3604, #9537, #14442 ) ) ;
#7671 = AXIS2_PLACEMENT_3D ( 'NONE', #4135, #7455, #9529 ) ;
#7672 = DIRECTION ( 'NONE',  ( -1.000000000000000000, 0.000000000000000000, 0.000000000000000000 ) ) ;
#7673 = ORIENTED_EDGE ( 'NONE', *, *, #12665, .F. ) ;
#7674 = CYLINDRICAL_SURFACE ( 'NONE', #2038, 44.99999999999998579 ) ;
#7675 = SURFACE_SIDE_STYLE ('',( #6138 ) ) ;
#7676 = EDGE_CURVE ( 'NONE', #289, #2742, #3276, .T. ) ;
#7677 = DIRECTION ( 'NONE',  ( -1.000000000000000000, -0.000000000000000000, -0.000000000000000000 ) ) ;
#7678 = ORIENTED_EDGE ( 'NONE', *, *, #342, .T. ) ;
#7679 = AXIS2_PLACEMENT_3D ( 'NONE', #3450, #18153, #9733 ) ;
#7680 = VERTEX_POINT ( 'NONE', #314 ) ;
#7681 = ORIENTED_EDGE ( 'NONE', *, *, #20558, .T. ) ;
#7682 = VERTEX_POINT ( 'NONE', #5497 ) ;
#7683 = VECTOR ( 'NONE', #18189, 1000.000000000000000 ) ;
#7684 = CARTESIAN_POINT ( 'NONE',  ( 10.00000000000000000, -21.31452625070873452, -82.34610137166143318 ) ) ;
#7685 = CARTESIAN_POINT ( 'NONE',  ( 10.00000000000000000, -51.76708072107842185, -67.49339815138544907 ) ) ;
#7686 = AXIS2_PLACEMENT_3D ( 'NONE', #3891, #5116, #366 ) ;
#7687 = ADVANCED_FACE ( 'NONE', ( #3728 ), #16992, .T. ) ;
#7688 = EDGE_LOOP ( 'NONE', ( #8821, #13823, #11187, #15691 ) ) ;
#7689 = CARTESIAN_POINT ( 'NONE',  ( 10.00000000000000000, 31.88200538760793634, 2.745493118647100772 ) ) ;
#7690 = DIRECTION ( 'NONE',  ( -1.000000000000000000, 0.000000000000000000, 0.000000000000000000 ) ) ;
#7691 = DIRECTION ( 'NONE',  ( -0.000000000000000000, -0.000000000000000000, -1.000000000000000000 ) ) ;
#7692 = CARTESIAN_POINT ( 'NONE',  ( 0.000000000000000000, 0.000000000000000000, 0.000000000000000000 ) ) ;
#7693 = AXIS2_PLACEMENT_3D ( 'NONE', #12170, #15260, #13937 ) ;
#7694 = LINE ( 'NONE', #952, #5557 ) ;
#7695 = ADVANCED_FACE ( 'NONE', ( #17424 ), #3613, .F. ) ;
#7696 = ORIENTED_EDGE ( 'NONE', *, *, #20676, .T. ) ;
#7697 = FACE_OUTER_BOUND ( 'NONE', #5911, .T. ) ;
#7698 = AXIS2_PLACEMENT_3D ( 'NONE', #21217, #10826, #16345 ) ;
#7699 = CIRCLE ( 'NONE', #9800, 88.00000000000000000 ) ;
#7700 = CARTESIAN_POINT ( 'NONE',  ( 10.00000000000000000, 0.000000000000000000, 0.000000000000000000 ) ) ;
#7701 = AXIS2_PLACEMENT_3D ( 'NONE', #1908, #8649, #15381 ) ;
#7702 = VECTOR ( 'NONE', #6211, 1000.000000000000000 ) ;
#7703 = CARTESIAN_POINT ( 'NONE',  ( 10.00000000000000000, -91.70173545986510533, -12.13370160540135423 ) ) ;
#7704 = ORIENTED_EDGE ( 'NONE', *, *, #21592, .T. ) ;
#7705 = EDGE_CURVE ( 'NONE', #2939, #419, #3969, .T. ) ;
#7706 = DIRECTION ( 'NONE',  ( -1.000000000000000000, 0.000000000000000000, 0.000000000000000000 ) ) ;
#7707 = EDGE_CURVE ( 'NONE', #10823, #14878, #4320, .T. ) ;
#7708 = ADVANCED_FACE ( 'NONE', ( #19085 ), #3941, .F. ) ;
#7709 = VERTEX_POINT ( 'NONE', #7149 ) ;
#7710 = CARTESIAN_POINT ( 'NONE',  ( -2.000000000000000000, 67.00000000000000000, 15.00000000000000000 ) ) ;
#7711 = EDGE_LOOP ( 'NONE', ( #12257, #18137, #1812, #20675 ) ) ;
#7712 = DIRECTION ( 'NONE',  ( 1.000000000000000000, 0.000000000000000000, 0.000000000000000000 ) ) ;
#7713 = EDGE_CURVE ( 'NONE', #14091, #8622, #16679, .T. ) ;
#7714 = ORIENTED_EDGE ( 'NONE', *, *, #19627, .F. ) ;
#7715 = ORIENTED_EDGE ( 'NONE', *, *, #19827, .T. ) ;
#7716 = CARTESIAN_POINT ( 'NONE',  ( 10.00000000000000000, -12.94633825542284278, 24.26081875733330406 ) ) ;
#7717 = VERTEX_POINT ( 'NONE', #8591 ) ;
#7718 = CARTESIAN_POINT ( 'NONE',  ( 10.00000000000000000, -79.66702613806795341, 29.80527447819410369 ) ) ;
#7719 = CIRCLE ( 'NONE', #8787, 44.99999999999999289 ) ;
#7720 = CARTESIAN_POINT ( 'NONE',  ( 0.000000000000000000, -21.69483248597410707, -16.89761061231802586 ) ) ;
#7721 = FACE_OUTER_BOUND ( 'NONE', #44, .T. ) ;
#7722 = AXIS2_PLACEMENT_3D ( 'NONE', #17112, #6962, #8718 ) ;
#7723 = AXIS2_PLACEMENT_3D ( 'NONE', #9712, #17917, #13256 ) ;
#7724 = AXIS2_PLACEMENT_3D ( 'NONE', #9389, #19131, #3994 ) ;
#7725 = DIRECTION ( 'NONE',  ( 0.000000000000000000, 0.9848077530122073542, 0.1736481776669339949 ) ) ;
#7726 = EDGE_CURVE ( 'NONE', #5530, #8987, #20901, .T. ) ;
#7727 = CARTESIAN_POINT ( 'NONE',  ( 0.000000000000000000, -35.18804927320473297, -80.65854690202716881 ) ) ;
#7728 = DIRECTION ( 'NONE',  ( 0.000000000000000000, -0.6946583704590034714, 0.7193398003386453077 ) ) ;
#7729 = DIRECTION ( 'NONE',  ( -1.000000000000000000, 0.000000000000000000, 0.000000000000000000 ) ) ;
#7730 = ADVANCED_FACE ( 'NONE', ( #15548 ), #3839, .T. ) ;
#7731 = CARTESIAN_POINT ( 'NONE',  ( 0.000000000000000000, 0.000000000000000000, 0.000000000000000000 ) ) ;
#7732 = CARTESIAN_POINT ( 'NONE',  ( 0.000000000000000000, 85.54350296776112828, 20.64725405482881726 ) ) ;
#7733 = CIRCLE ( 'NONE', #16201, 7.500000000000000000 ) ;
#7734 = ORIENTED_EDGE ( 'NONE', *, *, #18697, .T. ) ;
#7735 = AXIS2_PLACEMENT_3D ( 'NONE', #18323, #1621, #20296 ) ;
#7736 = VERTEX_POINT ( 'NONE', #11545 ) ;
#7737 = AXIS2_PLACEMENT_3D ( 'NONE', #2508, #8820, #15557 ) ;
#7738 = VECTOR ( 'NONE', #8615, 1000.000000000000000 ) ;
#7739 = ORIENTED_EDGE ( 'NONE', *, *, #4288, .T. ) ;
#7740 = EDGE_CURVE ( 'NONE', #20538, #9177, #10680, .T. ) ;
#7741 = EDGE_LOOP ( 'NONE', ( #19913, #7396, #15805, #21083 ) ) ;
#7742 = ORIENTED_EDGE ( 'NONE', *, *, #9594, .F. ) ;
#7743 = DIRECTION ( 'NONE',  ( 0.000000000000000000, 0.000000000000000000, 1.000000000000000000 ) ) ;
#7744 = ORIENTED_EDGE ( 'NONE', *, *, #3834, .T. ) ;
#7745 = DIRECTION ( 'NONE',  ( -1.000000000000000000, -0.000000000000000000, 0.000000000000000000 ) ) ;
#7746 = PLANE ( 'NONE',  #5514 ) ;
#7747 = DIRECTION ( 'NONE',  ( -1.000000000000000000, 0.000000000000000000, 0.000000000000000000 ) ) ;
#7748 = VECTOR ( 'NONE', #404, 1000.000000000000000 ) ;
#7749 = ADVANCED_FACE ( 'NONE', ( #13185 ), #9878, .F. ) ;
#7750 = DIRECTION ( 'NONE',  ( -1.000000000000000000, 0.000000000000000000, 0.000000000000000000 ) ) ;
#7751 = DIRECTION ( 'NONE',  ( 0.000000000000000000, 0.000000000000000000, 1.000000000000000000 ) ) ;
#7752 = VECTOR ( 'NONE', #14743, 1000.000000000000000 ) ;
#7753 = DIRECTION ( 'NONE',  ( 1.000000000000000000, 0.000000000000000000, 0.000000000000000000 ) ) ;
#7754 = CIRCLE ( 'NONE', #20458, 12.00000000000000178 ) ;
#7755 = EDGE_CURVE ( 'NONE', #15070, #20799, #2230, .T. ) ;
#7756 = CARTESIAN_POINT ( 'NONE',  ( 5.000000000000000000, 0.6021240089801385142, 31.99433460282945063 ) ) ;
#7757 = DIRECTION ( 'NONE',  ( 1.000000000000000000, 0.000000000000000000, 0.000000000000000000 ) ) ;
#7758 = DIRECTION ( 'NONE',  ( 0.000000000000000000, 0.000000000000000000, 1.000000000000000000 ) ) ;
#7759 = ADVANCED_FACE ( 'NONE', ( #3145 ), #3247, .F. ) ;
#7760 = ORIENTED_EDGE ( 'NONE', *, *, #2470, .T. ) ;
#7761 = EDGE_CURVE ( 'NONE', #17932, #2613, #13869, .T. ) ;
#7762 = ADVANCED_BREP_SHAPE_REPRESENTATION ( '', ( #13088, #15567 ), #19439 ) ;
#7763 = DIRECTION ( 'NONE',  ( 0.000000000000000000, 0.000000000000000000, 1.000000000000000000 ) ) ;
#7764 = ORIENTED_EDGE ( 'NONE', *, *, #19442, .T. ) ;
#7765 = CARTESIAN_POINT ( 'NONE',  ( 10.00000000000000000, -26.27606311335944511, -10.21217444509438188 ) ) ;
#7766 = CARTESIAN_POINT ( 'NONE',  ( 10.00000000000000000, 65.64563793391829449, 54.09103124042837862 ) ) ;
#7767 = VERTEX_POINT ( 'NONE', #4922 ) ;
#7768 = AXIS2_PLACEMENT_3D ( 'NONE', #16511, #14847, #21585 ) ;
#7769 = CYLINDRICAL_SURFACE ( 'NONE', #15714, 92.50100000000000477 ) ;
#7770 = VERTEX_POINT ( 'NONE', #6586 ) ;
#7771 = ORIENTED_EDGE ( 'NONE', *, *, #13279, .T. ) ;
#7772 = DIRECTION ( 'NONE',  ( 2.775557561562891351E-17, 1.000000000000000000, 2.081668171172168513E-16 ) ) ;
#7773 = DIRECTION ( 'NONE',  ( 0.000000000000000000, 0.000000000000000000, 1.000000000000000000 ) ) ;
#7774 = ORIENTED_EDGE ( 'NONE', *, *, #4193, .T. ) ;
#7775 = VERTEX_POINT ( 'NONE', #11978 ) ;
#7776 = LINE ( 'NONE', #1134, #4396 ) ;
#7777 = DIRECTION ( 'NONE',  ( -1.000000000000000000, -0.000000000000000000, 0.000000000000000000 ) ) ;
#7778 = DIRECTION ( 'NONE',  ( -1.000000000000000000, 0.000000000000000000, -0.000000000000000000 ) ) ;
#7779 = CARTESIAN_POINT ( 'NONE',  ( 0.000000000000000000, -25.17124263951018293, 12.69364185792209909 ) ) ;
#7780 = CARTESIAN_POINT ( 'NONE',  ( 1.114299999999999846, 6.898680348956876061E-16, 5.633200000000004870 ) ) ;
#7781 = CARTESIAN_POINT ( 'NONE',  ( 10.00000000000000000, 65.64563793391829449, 54.09103124042837862 ) ) ;
#7782 = CARTESIAN_POINT ( 'NONE',  ( 0.000000000000000000, 0.000000000000000000, 100.0000000000000000 ) ) ;
#7783 = DIRECTION ( 'NONE',  ( 1.000000000000000000, 0.000000000000000000, 0.000000000000000000 ) ) ;
#7784 = CARTESIAN_POINT ( 'NONE',  ( 10.00000000000000000, 0.000000000000000000, 0.000000000000000000 ) ) ;
#7785 = ORIENTED_EDGE ( 'NONE', *, *, #9726, .T. ) ;
#7786 = CARTESIAN_POINT ( 'NONE',  ( 10.00000000000000000, -81.32027326007897727, 44.08455690949027428 ) ) ;
#7787 = ORIENTED_EDGE ( 'NONE', *, *, #19896, .F. ) ;
#7788 = CARTESIAN_POINT ( 'NONE',  ( 10.00000000000000000, -30.61448696004458370, 9.314139153634121371 ) ) ;
#7789 = CARTESIAN_POINT ( 'NONE',  ( 8.899999999999989697, 0.000000000000000000, 0.000000000000000000 ) ) ;
#7790 = CYLINDRICAL_SURFACE ( 'NONE', #4214, 44.99999999999999289 ) ;
#7791 = ORIENTED_EDGE ( 'NONE', *, *, #10161, .T. ) ;
#7792 = VERTEX_POINT ( 'NONE', #50 ) ;
#7793 = VERTEX_POINT ( 'NONE', #16724 ) ;
#7794 = ORIENTED_EDGE ( 'NONE', *, *, #1917, .T. ) ;
#7795 = VECTOR ( 'NONE', #10283, 1000.000000000000000 ) ;
#7796 = CARTESIAN_POINT ( 'NONE',  ( 10.00000000000000000, 0.000000000000000000, 0.000000000000000000 ) ) ;
#7797 = DIRECTION ( 'NONE',  ( 0.000000000000000000, -0.7880107536067145757, -0.6156614753256675066 ) ) ;
#7798 = ORIENTED_EDGE ( 'NONE', *, *, #18556, .F. ) ;
#7799 = DIRECTION ( 'NONE',  ( -1.000000000000000000, -0.000000000000000000, -0.000000000000000000 ) ) ;
#7800 = DIRECTION ( 'NONE',  ( 0.000000000000000000, 0.000000000000000000, 1.000000000000000000 ) ) ;
#7801 = DIRECTION ( 'NONE',  ( 0.000000000000000000, 1.224646799147324364E-16, 1.000000000000000000 ) ) ;
#7802 = CARTESIAN_POINT ( 'NONE',  ( -90.00000000000000000, 1.224646799147353533E-14, 100.0000000000000284 ) ) ;
#7803 = DIRECTION ( 'NONE',  ( 0.000000000000000000, 0.2079116908177598144, -0.9781476007338055778 ) ) ;
#7804 = ADVANCED_FACE ( 'NONE', ( #1591 ), #8338, .F. ) ;
#7805 = EDGE_LOOP ( 'NONE', ( #6029, #16972, #21019, #3923 ) ) ;
#7806 = DIRECTION ( 'NONE',  ( -1.000000000000000000, 0.000000000000000000, 0.000000000000000000 ) ) ;
#7807 = CARTESIAN_POINT ( 'NONE',  ( 10.00000000000000000, 1.224646799147353217E-14, -100.0000000000000000 ) ) ;
#7808 = VERTEX_POINT ( 'NONE', #20381 ) ;
#7809 = ADVANCED_FACE ( 'NONE', ( #18726 ), #17059, .T. ) ;
#7810 = DIRECTION ( 'NONE',  ( -1.000000000000000000, -0.000000000000000000, -0.000000000000000000 ) ) ;
#7811 = ORIENTED_EDGE ( 'NONE', *, *, #14057, .F. ) ;
#7812 = FACE_OUTER_BOUND ( 'NONE', #1481, .T. ) ;
#7813 = CYLINDRICAL_SURFACE ( 'NONE', #17611, 45.00000000000000000 ) ;
#7814 = ORIENTED_EDGE ( 'NONE', *, *, #10385, .F. ) ;
#7815 = DIRECTION ( 'NONE',  ( 0.000000000000000000, -0.9510565162951502005, -0.3090169943749575543 ) ) ;
#7816 = EDGE_LOOP ( 'NONE', ( #20612, #5674, #6725, #355 ) ) ;
#7817 = ORIENTED_EDGE ( 'NONE', *, *, #17695, .F. ) ;
#7818 = CARTESIAN_POINT ( 'NONE',  ( 0.000000000000000000, 0.000000000000000000, 25.00000000000000000 ) ) ;
#7819 = ORIENTED_EDGE ( 'NONE', *, *, #5585, .F. ) ;
#7820 = FACE_OUTER_BOUND ( 'NONE', #20027, .T. ) ;
#7821 = CARTESIAN_POINT ( 'NONE',  ( 1.500000000000001332, 0.000000000000000000, 5.453125000000000000 ) ) ;
#7822 = FACE_OUTER_BOUND ( 'NONE', #7011, .T. ) ;
#7823 = DIRECTION ( 'NONE',  ( 1.000000000000000000, 0.000000000000000000, 0.000000000000000000 ) ) ;
#7824 = EDGE_CURVE ( 'NONE', #17747, #12605, #11039, .T. ) ;
#7825 = DIRECTION ( 'NONE',  ( 0.000000000000000000, -0.3420201433256569445, -0.9396926207859126468 ) ) ;
#7826 = EDGE_CURVE ( 'NONE', #3440, #8227, #18470, .T. ) ;
#7827 = CARTESIAN_POINT ( 'NONE',  ( 0.000000000000000000, -69.25892805976475586, -49.38005998797915908 ) ) ;
#7828 = EDGE_CURVE ( 'NONE', #14098, #6130, #6476, .T. ) ;
#7829 = LINE ( 'NONE', #17897, #21776 ) ;
#7830 = FACE_OUTER_BOUND ( 'NONE', #6585, .T. ) ;
#7831 = ADVANCED_FACE ( 'NONE', ( #6470 ), #10211, .F. ) ;
#7832 = DIRECTION ( 'NONE',  ( -1.000000000000000000, 0.000000000000000000, 0.000000000000000000 ) ) ;
#7833 = ORIENTED_EDGE ( 'NONE', *, *, #7154, .T. ) ;
#7834 = ORIENTED_EDGE ( 'NONE', *, *, #4633, .F. ) ;
#7835 = EDGE_LOOP ( 'NONE', ( #593, #21210, #20781, #9135 ) ) ;
#7836 = EDGE_CURVE ( 'NONE', #4275, #20304, #13502, .T. ) ;
#7837 = AXIS2_PLACEMENT_3D ( 'NONE', #18027, #4541, #4646 ) ;
#7838 = ORIENTED_EDGE ( 'NONE', *, *, #13457, .T. ) ;
#7839 = ORIENTED_EDGE ( 'NONE', *, *, #17, .T. ) ;
#7840 = EDGE_CURVE ( 'NONE', #5185, #10039, #19866, .T. ) ;
#7841 = CYLINDRICAL_SURFACE ( 'NONE', #18658, 92.50100000000000477 ) ;
#7842 = VECTOR ( 'NONE', #21113, 1000.000000000000000 ) ;
#7843 = ORIENTED_EDGE ( 'NONE', *, *, #15969, .F. ) ;
#7844 = LINE ( 'NONE', #3905, #4303 ) ;
#7845 = CARTESIAN_POINT ( 'NONE',  ( 9.999999999999994671, 0.000000000000000000, 0.000000000000000000 ) ) ;
#7846 = AXIS2_PLACEMENT_3D ( 'NONE', #18979, #20526, #18870 ) ;
#7847 = DIRECTION ( 'NONE',  ( 1.000000000000000000, 0.000000000000000000, 0.000000000000000000 ) ) ;
#7848 = CARTESIAN_POINT ( 'NONE',  ( 10.00000000000000000, 0.000000000000000000, 0.000000000000000000 ) ) ;
#7849 = CYLINDRICAL_SURFACE ( 'NONE', #9753, 88.00000000000000000 ) ;
#7850 = EDGE_CURVE ( 'NONE', #11042, #15057, #14926, .T. ) ;
#7851 = CARTESIAN_POINT ( 'NONE',  ( 10.00000000000000000, -92.49798535263882115, -0.7467976319030308341 ) ) ;
#7852 = LINE ( 'NONE', #9831, #11534 ) ;
#7853 = CARTESIAN_POINT ( 'NONE',  ( 10.00000000000000000, -31.15801000616779248, -79.14775961996421927 ) ) ;
#7854 = EDGE_CURVE ( 'NONE', #12163, #6716, #18614, .T. ) ;
#7855 = AXIS2_PLACEMENT_3D ( 'NONE', #544, #20766, #20650 ) ;
#7856 = ORIENTED_EDGE ( 'NONE', *, *, #8934, .F. ) ;
#7857 = CARTESIAN_POINT ( 'NONE',  ( 10.00000000000000000, -56.35896156214896280, -73.34918167666369015 ) ) ;
#7858 = AXIS2_PLACEMENT_3D ( 'NONE', #8183, #13469, #1547 ) ;
#7859 = AXIS2_PLACEMENT_3D ( 'NONE', #6969, #8725, #648 ) ;
#7860 = EDGE_LOOP ( 'NONE', ( #6961, #14275 ) ) ;
#7861 = AXIS2_PLACEMENT_3D ( 'NONE', #2076, #1852, #13675 ) ;
#7862 = DIRECTION ( 'NONE',  ( -1.000000000000000000, -0.000000000000000000, 0.000000000000000000 ) ) ;
#7863 = EDGE_CURVE ( 'NONE', #19313, #9664, #156, .T. ) ;
#7864 = CARTESIAN_POINT ( 'NONE',  ( 0.000000000000000000, 65.64563793391829449, 54.09103124042837862 ) ) ;
#7865 = AXIS2_PLACEMENT_3D ( 'NONE', #10619, #17367, #2222 ) ;
#7866 = ORIENTED_EDGE ( 'NONE', *, *, #6361, .F. ) ;
#7867 = CARTESIAN_POINT ( 'NONE',  ( 10.00000000000000000, 36.39558101400137957, 80.12091913260394449 ) ) ;
#7868 = ORIENTED_EDGE ( 'NONE', *, *, #6069, .F. ) ;
#7869 = EDGE_CURVE ( 'NONE', #173, #18557, #8972, .T. ) ;
#7870 = ORIENTED_EDGE ( 'NONE', *, *, #29, .F. ) ;
#7871 =( NAMED_UNIT ( * ) PLANE_ANGLE_UNIT ( ) SI_UNIT ( $, .RADIAN. ) );
#7872 = CARTESIAN_POINT ( 'NONE',  ( 8.899999999999991473, 0.000000000000000000, 0.000000000000000000 ) ) ;
#7873 = AXIS2_PLACEMENT_3D ( 'NONE', #14672, #12461, #2629 ) ;
#7874 = VERTEX_POINT ( 'NONE', #4007 ) ;
#7875 = ORIENTED_EDGE ( 'NONE', *, *, #3004, .T. ) ;
#7876 = EDGE_CURVE ( 'NONE', #17373, #17077, #3981, .T. ) ;
#7877 = CARTESIAN_POINT ( 'NONE',  ( 10.00000000000000000, -25.48117629651182270, -10.33947075754286793 ) ) ;
#7878 = DIRECTION ( 'NONE',  ( 0.000000000000000000, 0.000000000000000000, 1.000000000000000000 ) ) ;
#7879 = EDGE_CURVE ( 'NONE', #20207, #8011, #10333, .T. ) ;
#7880 = AXIS2_PLACEMENT_3D ( 'NONE', #13969, #12517, #602 ) ;
#7881 = CARTESIAN_POINT ( 'NONE',  ( 10.00000000000000000, 6.063030049135075039, 31.42037024962127134 ) ) ;
#7882 = DIRECTION ( 'NONE',  ( 1.000000000000000000, 0.000000000000000000, -0.000000000000000000 ) ) ;
#7883 = LINE ( 'NONE', #8206, #10441 ) ;
#7884 = CARTESIAN_POINT ( 'NONE',  ( 0.000000000000000000, -62.44821182181136976, 68.23969402963483333 ) ) ;
#7885 = CYLINDRICAL_SURFACE ( 'NONE', #497, 92.50100000000000477 ) ;
#7886 = LINE ( 'NONE', #14403, #11947 ) ;
#7887 = DIRECTION ( 'NONE',  ( -1.000000000000000000, 0.000000000000000000, 0.000000000000000000 ) ) ;
#7888 = EDGE_CURVE ( 'NONE', #21408, #11959, #18816, .T. ) ;
#7889 = ORIENTED_EDGE ( 'NONE', *, *, #11162, .F. ) ;
#7890 = DIRECTION ( 'NONE',  ( 1.000000000000000000, -0.000000000000000000, -0.000000000000000000 ) ) ;
#7891 = VECTOR ( 'NONE', #14536, 1000.000000000000000 ) ;
#7892 = VERTEX_POINT ( 'NONE', #8868 ) ;
#7893 = LINE ( 'NONE', #8214, #16863 ) ;
#7894 = AXIS2_PLACEMENT_3D ( 'NONE', #9101, #12631, #15618 ) ;
#7895 = CARTESIAN_POINT ( 'NONE',  ( 10.00000000000000000, 0.000000000000000000, 0.000000000000000000 ) ) ;
#7896 = ORIENTED_EDGE ( 'NONE', *, *, #20433, .F. ) ;
#7897 = AXIS2_PLACEMENT_3D ( 'NONE', #6731, #13664, #18433 ) ;
#7898 = SURFACE_STYLE_USAGE ( .BOTH. , #4361 ) ;
#7899 = EDGE_LOOP ( 'NONE', ( #3703, #6906, #39, #17953 ) ) ;
#7900 = EDGE_LOOP ( 'NONE', ( #424, #6643, #20073, #1715 ) ) ;
#7901 = ORIENTED_EDGE ( 'NONE', *, *, #6517, .F. ) ;
#7902 = DIRECTION ( 'NONE',  ( -1.000000000000000000, 0.000000000000000000, -0.000000000000000000 ) ) ;
#7903 = CARTESIAN_POINT ( 'NONE',  ( 0.000000000000000000, -37.96946988134122591, -76.11510229470897571 ) ) ;
#7904 = EDGE_LOOP ( 'NONE', ( #8313, #13463, #13974, #18147 ) ) ;
#7905 = EDGE_CURVE ( 'NONE', #20271, #1347, #18106, .T. ) ;
#7906 = AXIS2_PLACEMENT_3D ( 'NONE', #12434, #12547, #14317 ) ;
#7907 = CYLINDRICAL_SURFACE ( 'NONE', #11807, 11.99999999999999822 ) ;
#7908 = DIRECTION ( 'NONE',  ( 0.000000000000000000, 0.000000000000000000, 1.000000000000000000 ) ) ;
#7909 = DIRECTION ( 'NONE',  ( 1.000000000000000000, -0.000000000000000000, -0.000000000000000000 ) ) ;
#7910 = CARTESIAN_POINT ( 'NONE',  ( 10.00000000000000000, 0.000000000000000000, 0.000000000000000000 ) ) ;
#7911 = CARTESIAN_POINT ( 'NONE',  ( 10.00000000000000000, 92.49798535263882115, 0.7467976319023850174 ) ) ;
#7912 = UNCERTAINTY_MEASURE_WITH_UNIT (LENGTH_MEASURE( 1.000000000000000082E-05 ), #3205, 'distance_accuracy_value', 'NONE');
#7913 = AXIS2_PLACEMENT_3D ( 'NONE', #2827, #11221, #21502 ) ;
#7914 = ORIENTED_EDGE ( 'NONE', *, *, #11893, .T. ) ;
#7915 = AXIS2_PLACEMENT_3D ( 'NONE', #3475, #8341, #15180 ) ;
#7916 = CARTESIAN_POINT ( 'NONE',  ( 10.00000000000000000, -90.63195040374174027, -18.50093422002511900 ) ) ;
#7917 = CARTESIAN_POINT ( 'NONE',  ( 10.00000000000000000, 21.31452625071037943, -82.34610137166097843 ) ) ;
#7918 = ORIENTED_EDGE ( 'NONE', *, *, #4971, .T. ) ;
#7919 = DIRECTION ( 'NONE',  ( 0.000000000000000000, 0.3420201433256694901, -0.9396926207859080948 ) ) ;
#7920 = ORIENTED_EDGE ( 'NONE', *, *, #12107, .F. ) ;
#7921 = AXIS2_PLACEMENT_3D ( 'NONE', #14646, #21393, #1286 ) ;
#7922 = DIRECTION ( 'NONE',  ( -1.000000000000000000, 0.000000000000000000, 0.000000000000000000 ) ) ;
#7923 = DIRECTION ( 'NONE',  ( 0.000000000000000000, -0.7880107536067275653, 0.6156614753256510753 ) ) ;
#7924 = EDGE_LOOP ( 'NONE', ( #8411, #7465, #12128, #12619 ) ) ;
#7925 = DIRECTION ( 'NONE',  ( -0.000000000000000000, 0.000000000000000000, 1.000000000000000000 ) ) ;
#7926 = CIRCLE ( 'NONE', #7238, 7.500000000000000000 ) ;
#7927 = ORIENTED_EDGE ( 'NONE', *, *, #7836, .F. ) ;
#7928 = EDGE_CURVE ( 'NONE', #20507, #454, #9607, .T. ) ;
#7929 = ORIENTED_EDGE ( 'NONE', *, *, #15303, .T. ) ;
#7930 = CARTESIAN_POINT ( 'NONE',  ( 10.00000000000000000, 78.01214607583800387, -33.90124636420030413 ) ) ;
#7931 = AXIS2_PLACEMENT_3D ( 'NONE', #7660, #18155, #3011 ) ;
#7932 = VERTEX_POINT ( 'NONE', #17173 ) ;
#7933 = DIRECTION ( 'NONE',  ( 0.000000000000000000, 0.000000000000000000, 1.000000000000000000 ) ) ;
#7934 = DIRECTION ( 'NONE',  ( 0.000000000000000000, 0.000000000000000000, 1.000000000000000000 ) ) ;
#7935 = CARTESIAN_POINT ( 'NONE',  ( 10.00000000000000000, 1.592605004253184964, -28.14575649959892445 ) ) ;
#7936 = DIRECTION ( 'NONE',  ( 0.000000000000000000, 0.000000000000000000, 1.000000000000000000 ) ) ;
#7937 = EDGE_CURVE ( 'NONE', #19662, #16982, #16690, .T. ) ;
#7938 = CIRCLE ( 'NONE', #8976, 11.99999999999999645 ) ;
#7939 = CARTESIAN_POINT ( 'NONE',  ( 0.000000000000000000, -27.26034713664092379, -7.182859710736426706 ) ) ;
#7940 = CYLINDRICAL_SURFACE ( 'NONE', #9250, 92.50100000000000477 ) ;
#7941 = AXIS2_PLACEMENT_3D ( 'NONE', #3288, #3402, #20197 ) ;
#7942 = LINE ( 'NONE', #18009, #11552 ) ;
#7943 = DIRECTION ( 'NONE',  ( 0.000000000000000000, 0.4067366430758010409, -0.9135454576426005335 ) ) ;
#7944 = AXIS2_PLACEMENT_3D ( 'NONE', #18806, #8318, #16704 ) ;
#7945 = DIRECTION ( 'NONE',  ( 1.000000000000000000, 0.000000000000000000, 0.000000000000000000 ) ) ;
#7946 = CIRCLE ( 'NONE', #12502, 11.99999999999999822 ) ;
#7947 = DIRECTION ( 'NONE',  ( -1.000000000000000000, -0.000000000000000000, -0.000000000000000000 ) ) ;
#7948 = EDGE_LOOP ( 'NONE', ( #4008, #18047, #16319, #5513 ) ) ;
#7949 = ORIENTED_EDGE ( 'NONE', *, *, #17215, .T. ) ;
#7950 = ORIENTED_EDGE ( 'NONE', *, *, #423, .F. ) ;
#7951 = ORIENTED_EDGE ( 'NONE', *, *, #17163, .F. ) ;
#7952 = EDGE_CURVE ( 'NONE', #5893, #4745, #12396, .T. ) ;
#7953 = AXIS2_PLACEMENT_3D ( 'NONE', #1500, #11563, #19955 ) ;
#7954 = AXIS2_PLACEMENT_3D ( 'NONE', #3678, #3575, #10205 ) ;
#7955 = CIRCLE ( 'NONE', #21362, 0.2042000000000016025 ) ;
#7956 = ORIENTED_EDGE ( 'NONE', *, *, #3615, .T. ) ;
#7957 = CARTESIAN_POINT ( 'NONE',  ( 10.00000000000000000, 0.000000000000000000, 0.000000000000000000 ) ) ;
#7958 = ORIENTED_EDGE ( 'NONE', *, *, #6756, .T. ) ;
#7959 = CARTESIAN_POINT ( 'NONE',  ( 10.00000000000000000, -8.925965667929485647, 92.06933331948778232 ) ) ;
#7960 = DIRECTION ( 'NONE',  ( 0.000000000000000000, 0.4694715627858916940, -0.8829475928589264333 ) ) ;
#7961 = DIRECTION ( 'NONE',  ( -1.000000000000000000, 0.000000000000000000, 0.000000000000000000 ) ) ;
#7962 = DIRECTION ( 'NONE',  ( 1.000000000000000000, 0.000000000000000000, 0.000000000000000000 ) ) ;
#7963 = DIRECTION ( 'NONE',  ( 0.000000000000000000, 0.000000000000000000, 1.000000000000000000 ) ) ;
#7964 = AXIS2_PLACEMENT_3D ( 'NONE', #11643, #15163, #6458 ) ;
#7965 = CARTESIAN_POINT ( 'NONE',  ( 5.000000000000002665, 87.92084725184953697, -3.731570516142035387 ) ) ;
#7966 = ADVANCED_FACE ( 'NONE', ( #15839 ), #19046, .F. ) ;
#7967 = DIRECTION ( 'NONE',  ( 1.000000000000000000, 0.000000000000000000, 0.000000000000000000 ) ) ;
#7968 = AXIS2_PLACEMENT_3D ( 'NONE', #1229, #7972, #4318 ) ;
#7969 = ORIENTED_EDGE ( 'NONE', *, *, #3245, .F. ) ;
#7970 = AXIS2_PLACEMENT_3D ( 'NONE', #4250, #7672, #14406 ) ;
#7971 = AXIS2_PLACEMENT_3D ( 'NONE', #917, #21152, #19152 ) ;
#7972 = DIRECTION ( 'NONE',  ( -1.000000000000000000, -0.000000000000000000, -0.000000000000000000 ) ) ;
#7973 = CIRCLE ( 'NONE', #19981, 0.2042000000000016025 ) ;
#7974 = ORIENTED_EDGE ( 'NONE', *, *, #17837, .F. ) ;
#7975 = ORIENTED_EDGE ( 'NONE', *, *, #11192, .T. ) ;
#7976 = DIRECTION ( 'NONE',  ( 0.000000000000000000, -0.6427876096865458022, 0.7660444431189726844 ) ) ;
#7977 = CARTESIAN_POINT ( 'NONE',  ( 0.000000000000000000, 0.000000000000000000, -3.000000000000000000 ) ) ;
#7978 = ADVANCED_FACE ( 'NONE', ( #592 ), #5781, .T. ) ;
#7979 = EDGE_LOOP ( 'NONE', ( #17854, #17461, #13010, #13718 ) ) ;
#7980 = EDGE_CURVE ( 'NONE', #5374, #17052, #20235, .T. ) ;
#7981 = EDGE_CURVE ( 'NONE', #12259, #2865, #15269, .T. ) ;
#7982 = FACE_OUTER_BOUND ( 'NONE', #426, .T. ) ;
#7983 = ORIENTED_EDGE ( 'NONE', *, *, #17821, .T. ) ;
#7984 = ORIENTED_EDGE ( 'NONE', *, *, #19959, .T. ) ;
#7985 = DIRECTION ( 'NONE',  ( 1.000000000000000000, 0.000000000000000000, 0.000000000000000000 ) ) ;
#7986 = AXIS2_PLACEMENT_3D ( 'NONE', #3993, #9504, #7526 ) ;
#7987 = DIRECTION ( 'NONE',  ( -1.000000000000000000, 0.000000000000000000, 0.000000000000000000 ) ) ;
#7988 = EDGE_CURVE ( 'NONE', #14447, #2288, #12101, .T. ) ;
#7989 = ORIENTED_EDGE ( 'NONE', *, *, #16793, .T. ) ;
#7990 = CIRCLE ( 'NONE', #4105, 44.99999999999999289 ) ;
#7991 = ORIENTED_EDGE ( 'NONE', *, *, #17997, .F. ) ;
#7992 = CARTESIAN_POINT ( 'NONE',  ( 10.00000000000000000, -21.98203405400942856, -17.64965094506566246 ) ) ;
#7993 = VECTOR ( 'NONE', #18920, 1000.000000000000000 ) ;
#7994 = CARTESIAN_POINT ( 'NONE',  ( 10.00000000000000000, 0.000000000000000000, 0.000000000000000000 ) ) ;
#7995 = CARTESIAN_POINT ( 'NONE',  ( -1.500346250137462226E-14, 60.00000000000001421, 0.000000000000000000 ) ) ;
#7996 = LINE ( 'NONE', #21471, #18294 ) ;
#7997 = DIRECTION ( 'NONE',  ( 1.000000000000000000, 0.000000000000000000, 0.000000000000000000 ) ) ;
#7998 = CARTESIAN_POINT ( 'NONE',  ( 0.000000000000000000, -1.592605004252595213, -28.14575649959895998 ) ) ;
#7999 = DIRECTION ( 'NONE',  ( 0.000000000000000000, 0.000000000000000000, 1.000000000000000000 ) ) ;
#8000 = CARTESIAN_POINT ( 'NONE',  ( -10.00000000000000000, 0.000000000000000000, 0.000000000000000000 ) ) ;
#8001 = EDGE_CURVE ( 'NONE', #14362, #9395, #472, .T. ) ;
#8002 = DIRECTION ( 'NONE',  ( 0.000000000000000000, 0.000000000000000000, -1.000000000000000000 ) ) ;
#8003 = VERTEX_POINT ( 'NONE', #2029 ) ;
#8004 = EDGE_CURVE ( 'NONE', #21544, #3268, #8575, .T. ) ;
#8005 = ORIENTED_EDGE ( 'NONE', *, *, #5585, .T. ) ;
#8006 = AXIS2_PLACEMENT_3D ( 'NONE', #8595, #5394, #12234 ) ;
#8007 = EDGE_CURVE ( 'NONE', #19853, #7490, #1871, .T. ) ;
#8008 = CARTESIAN_POINT ( 'NONE',  ( 10.00000000000000000, 31.15801000616834315, 79.14775961996400611 ) ) ;
#8009 = DIRECTION ( 'NONE',  ( 1.000000000000000000, 0.000000000000000000, 0.000000000000000000 ) ) ;
#8010 = DIRECTION ( 'NONE',  ( 1.000000000000000000, 0.000000000000000000, 0.000000000000000000 ) ) ;
#8011 = VERTEX_POINT ( 'NONE', #12076 ) ;
#8012 = FILL_AREA_STYLE ('',( #933 ) ) ;
#8013 = VERTEX_POINT ( 'NONE', #5350 ) ;
#8014 = ADVANCED_FACE ( 'NONE', ( #17382 ), #18827, .T. ) ;
#8015 = ORIENTED_EDGE ( 'NONE', *, *, #19752, .T. ) ;
#8016 = ORIENTED_EDGE ( 'NONE', *, *, #1917, .F. ) ;
#8017 = DIRECTION ( 'NONE',  ( -1.000000000000000000, 0.000000000000000000, 0.000000000000000000 ) ) ;
#8018 = DIRECTION ( 'NONE',  ( -1.000000000000000000, 0.000000000000000000, 0.000000000000000000 ) ) ;
#8019 = VERTEX_POINT ( 'NONE', #12617 ) ;
#8020 = VECTOR ( 'NONE', #686, 1000.000000000000000 ) ;
#8021 = DIRECTION ( 'NONE',  ( -1.000000000000000000, 0.000000000000000000, 0.000000000000000000 ) ) ;
#8022 = FACE_BOUND ( 'NONE', #19747, .T. ) ;
#8023 = AXIS2_PLACEMENT_3D ( 'NONE', #5295, #320, #10682 ) ;
#8024 = CARTESIAN_POINT ( 'NONE',  ( -126.5000000000000000, 1.549178200921401833E-14, 25.00000000000000000 ) ) ;
#8025 = DIRECTION ( 'NONE',  ( -0.000000000000000000, -1.000000000000000000, -0.000000000000000000 ) ) ;
#8026 = AXIS2_PLACEMENT_3D ( 'NONE', #1313, #16229, #19534 ) ;
#8027 = DIRECTION ( 'NONE',  ( 1.000000000000000000, 0.000000000000000000, 0.000000000000000000 ) ) ;
#8028 = LINE ( 'NONE', #10106, #18739 ) ;
#8029 = ORIENTED_EDGE ( 'NONE', *, *, #1093, .F. ) ;
#8030 = EDGE_CURVE ( 'NONE', #11017, #21218, #4331, .T. ) ;
#8031 = CARTESIAN_POINT ( 'NONE',  ( 10.00000000000000000, -27.48365448817206058, -0.9185515634844814148 ) ) ;
#8032 = CARTESIAN_POINT ( 'NONE',  ( 1.200000000000006617, 0.000000000000000000, -5.612499999999999822 ) ) ;
#8033 = ORIENTED_EDGE ( 'NONE', *, *, #15656, .T. ) ;
#8034 = EDGE_CURVE ( 'NONE', #15305, #14192, #17609, .T. ) ;
#8035 = EDGE_CURVE ( 'NONE', #2943, #428, #20937, .T. ) ;
#8036 = LINE ( 'NONE', #5039, #5541 ) ;
#8037 = ORIENTED_EDGE ( 'NONE', *, *, #5938, .F. ) ;
#8038 = AXIS2_PLACEMENT_3D ( 'NONE', #4525, #2963, #11355 ) ;
#8039 = CARTESIAN_POINT ( 'NONE',  ( 0.000000000000000000, 0.000000000000000000, -88.00000000000000000 ) ) ;
#8040 = AXIS2_PLACEMENT_3D ( 'NONE', #817, #7561, #14295 ) ;
#8041 = TOROIDAL_SURFACE ( 'NONE', #20391, 7.400000000000019895, 0.1000000000000006994 ) ;
#8042 = DIRECTION ( 'NONE',  ( -1.000000000000000000, 0.000000000000000000, 0.000000000000000000 ) ) ;
#8043 = VECTOR ( 'NONE', #14460, 1000.000000000000000 ) ;
#8044 = ORIENTED_EDGE ( 'NONE', *, *, #15811, .F. ) ;
#8045 = CARTESIAN_POINT ( 'NONE',  ( -1.500000000000000666, 6.728125000000022560, 0.000000000000000000 ) ) ;
#8046 = ORIENTED_EDGE ( 'NONE', *, *, #6024, .F. ) ;
#8047 = VERTEX_POINT ( 'NONE', #1026 ) ;
#8048 = CYLINDRICAL_SURFACE ( 'NONE', #3405, 44.99999999999999289 ) ;
#8049 = ORIENTED_EDGE ( 'NONE', *, *, #13154, .F. ) ;
#8050 = DIRECTION ( 'NONE',  ( -1.000000000000000000, 0.000000000000000000, 0.000000000000000000 ) ) ;
#8051 = CARTESIAN_POINT ( 'NONE',  ( 1.500000000000001332, 0.000000000000000000, -6.728125000000023448 ) ) ;
#8052 = LINE ( 'NONE', #9796, #8925 ) ;
#8053 = CARTESIAN_POINT ( 'NONE',  ( 5.000000000000002665, -6.797690662954623875, -87.73705831432221203 ) ) ;
#8054 = CIRCLE ( 'NONE', #9799, 2.799999999999996714 ) ;
#8055 = AXIS2_PLACEMENT_3D ( 'NONE', #6569, #3338, #18051 ) ;
#8056 = CIRCLE ( 'NONE', #1344, 5.000000000000000000 ) ;
#8057 = CARTESIAN_POINT ( 'NONE',  ( 0.000000000000000000, -31.88200538760792213, -2.745493118647326369 ) ) ;
#8058 = DIRECTION ( 'NONE',  ( 1.000000000000000000, 0.000000000000000000, 0.000000000000000000 ) ) ;
#8059 = AXIS2_PLACEMENT_3D ( 'NONE', #19729, #21821, #6480 ) ;
#8060 = AXIS2_PLACEMENT_3D ( 'NONE', #12742, #10463, #2691 ) ;
#8061 = DIRECTION ( 'NONE',  ( -1.000000000000000000, 0.000000000000000000, 0.000000000000000000 ) ) ;
#8062 = DIRECTION ( 'NONE',  ( -1.000000000000000000, -0.000000000000000000, -0.000000000000000000 ) ) ;
#8063 = CARTESIAN_POINT ( 'NONE',  ( 10.00000000000000000, -19.83954325428602061, -82.71385593638713374 ) ) ;
#8064 = CARTESIAN_POINT ( 'NONE',  ( 10.00000000000000000, 19.07277123396568896, -19.80970465344728737 ) ) ;
#8065 = EDGE_LOOP ( 'NONE', ( #11725, #2678, #877, #13458 ) ) ;
#8066 = EDGE_LOOP ( 'NONE', ( #19417, #4065, #16313, #19579 ) ) ;
#8067 = ORIENTED_EDGE ( 'NONE', *, *, #15120, .T. ) ;
#8068 = VERTEX_POINT ( 'NONE', #4450 ) ;
#8069 = VECTOR ( 'NONE', #17228, 1000.000000000000000 ) ;
#8070 = AXIS2_PLACEMENT_3D ( 'NONE', #6771, #5186, #11919 ) ;
#8071 = ORIENTED_EDGE ( 'NONE', *, *, #18556, .T. ) ;
#8072 = DIRECTION ( 'NONE',  ( 1.000000000000000000, 0.000000000000000000, 0.000000000000000000 ) ) ;
#8073 = ORIENTED_EDGE ( 'NONE', *, *, #6500, .T. ) ;
#8074 = DIRECTION ( 'NONE',  ( -1.000000000000000000, -0.000000000000000000, -0.000000000000000000 ) ) ;
#8075 = LINE ( 'NONE', #5084, #4333 ) ;
#8076 = CARTESIAN_POINT ( 'NONE',  ( 10.00000000000000000, -46.89573839703331259, 79.73220629831473616 ) ) ;
#8077 = DIRECTION ( 'NONE',  ( -1.000000000000000000, 0.000000000000000000, -0.000000000000000000 ) ) ;
#8078 = CARTESIAN_POINT ( 'NONE',  ( 10.00000000000000000, 12.90135963484197212, -87.04915231966633371 ) ) ;
#8079 = VECTOR ( 'NONE', #2832, 1000.000000000000000 ) ;
#8080 = CARTESIAN_POINT ( 'NONE',  ( 5.000000000000002665, -85.22372865846305956, 21.92979875759598585 ) ) ;
#8081 = DIRECTION ( 'NONE',  ( 0.000000000000000000, -0.9510565162951565288, 0.3090169943749382364 ) ) ;
#8082 = EDGE_CURVE ( 'NONE', #2668, #8737, #12462, .T. ) ;
#8083 = AXIS2_PLACEMENT_3D ( 'NONE', #19639, #1181, #7923 ) ;
#8084 = TOROIDAL_SURFACE ( 'NONE', #7737, 5.100000000000000533, 0.1000000000000000472 ) ;
#8085 = VERTEX_POINT ( 'NONE', #11296 ) ;
#8087 = AXIS2_PLACEMENT_3D ( 'NONE', #12368, #2636, #9369 ) ;
#8086 = PRODUCT ( 'spur gear_iso_ISO - Spur gear 2M 30T 20PA 10FW ---S30B10H150L6.0S1', 'spur gear_iso_ISO - Spur gear 2M 30T 20PA 10FW ---S30B10H150L6.0S1', '', ( #3555 ) ) ;
#8088 = LINE ( 'NONE', #18582, #12902 ) ;
#8089 = VERTEX_POINT ( 'NONE', #12728 ) ;
#8090 = EDGE_CURVE ( 'NONE', #8367, #14246, #14594, .T. ) ;
#8091 = EDGE_LOOP ( 'NONE', ( #20759, #854 ) ) ;
#8092 = CARTESIAN_POINT ( 'NONE',  ( 10.00000000000000000, 27.48365448817206769, -0.9185515634842869037 ) ) ;
#8093 = ORIENTED_EDGE ( 'NONE', *, *, #10492, .T. ) ;
#8094 = DIRECTION ( 'NONE',  ( -1.000000000000000000, 0.000000000000000000, 0.000000000000000000 ) ) ;
#8095 = ORIENTED_EDGE ( 'NONE', *, *, #13959, .T. ) ;
#8096 = VERTEX_POINT ( 'NONE', #2896 ) ;
#8097 = ITEM_DEFINED_TRANSFORMATION ( 'NONE', 'NONE', #9930,  #15567 ) ;
#8098 = AXIS2_PLACEMENT_3D ( 'NONE', #1421, #18435, #18002 ) ;
#8099 = DIRECTION ( 'NONE',  ( 0.000000000000000000, 0.000000000000000000, -1.000000000000000000 ) ) ;
#8100 = ORIENTED_EDGE ( 'NONE', *, *, #207, .T. ) ;
#8101 = CARTESIAN_POINT ( 'NONE',  ( 0.000000000000000000, 6.123233995736766282E-16, 5.000000000000000000 ) ) ;
#8102 = AXIS2_PLACEMENT_3D ( 'NONE', #10004, #16747, #1834 ) ;
#8103 = CIRCLE ( 'NONE', #17282, 88.00000000000000000 ) ;
#8104 = CARTESIAN_POINT ( 'NONE',  ( 0.000000000000000000, -75.27139873020848881, -53.76477968147889896 ) ) ;
#8105 = CARTESIAN_POINT ( 'NONE',  ( 0.000000000000000000, 4.294029059349855793, 27.86182539015968018 ) ) ;
#8106 = CARTESIAN_POINT ( 'NONE',  ( 10.00000000000000000, -29.29369617358527833, 87.74003855418389719 ) ) ;
#8107 = CARTESIAN_POINT ( 'NONE',  ( 5.000000000000000000, 72.58367602204255320, -49.75550195834793499 ) ) ;
#8108 = FACE_OUTER_BOUND ( 'NONE', #635, .T. ) ;
#8109 = CARTESIAN_POINT ( 'NONE',  ( 0.000000000000000000, -27.48365448817207479, 0.9185515634840949462 ) ) ;
#8110 = DIRECTION ( 'NONE',  ( 1.000000000000000000, 0.000000000000000000, -0.000000000000000000 ) ) ;
#8111 = DIRECTION ( 'NONE',  ( 0.000000000000000000, 0.000000000000000000, 1.000000000000000000 ) ) ;
#8112 = EDGE_CURVE ( 'NONE', #13772, #1807, #10964, .T. ) ;
#8113 = ADVANCED_FACE ( 'NONE', ( #17711 ), #9292, .F. ) ;
#8114 = EDGE_CURVE ( 'NONE', #1263, #17806, #9279, .T. ) ;
#8115 = EDGE_LOOP ( 'NONE', ( #2327, #17201, #21285, #21104 ) ) ;
#8116 = ADVANCED_FACE ( 'NONE', ( #906 ), #19693, .F. ) ;
#8117 = ORIENTED_EDGE ( 'NONE', *, *, #14688, .T. ) ;
#8118 = CIRCLE ( 'NONE', #14413, 44.99999999999999289 ) ;
#8119 = DIRECTION ( 'NONE',  ( -1.000000000000000000, 0.000000000000000000, 0.000000000000000000 ) ) ;
#8120 = CARTESIAN_POINT ( 'NONE',  ( -1.399999999999998579, 0.000000000000000000, -5.000000000000000888 ) ) ;
#8121 = VERTEX_POINT ( 'NONE', #21464 ) ;
#8122 = DIRECTION ( 'NONE',  ( -1.000000000000000000, 0.000000000000000000, -0.000000000000000000 ) ) ;
#8123 = ORIENTED_EDGE ( 'NONE', *, *, #17967, .F. ) ;
#8124 = EDGE_CURVE ( 'NONE', #19281, #10630, #7657, .T. ) ;
#8125 = VERTEX_POINT ( 'NONE', #14503 ) ;
#8126 = DIRECTION ( 'NONE',  ( -1.000000000000000000, 0.000000000000000000, 0.000000000000000000 ) ) ;
#8127 = ORIENTED_EDGE ( 'NONE', *, *, #5067, .F. ) ;
#8128 = EDGE_LOOP ( 'NONE', ( #18421, #15143 ) ) ;
#8129 = CYLINDRICAL_SURFACE ( 'NONE', #6160, 11.99999999999999645 ) ;
#8130 = DIRECTION ( 'NONE',  ( -1.000000000000000000, -0.000000000000000000, -0.000000000000000000 ) ) ;
#8131 = ORIENTED_EDGE ( 'NONE', *, *, #16764, .T. ) ;
#8132 = EDGE_CURVE ( 'NONE', #5399, #5100, #6014, .T. ) ;
#8133 = CARTESIAN_POINT ( 'NONE',  ( 10.00000000000000000, -15.51843147776405729, 83.63233659819645993 ) ) ;
#8134 = DIRECTION ( 'NONE',  ( 0.000000000000000000, 0.000000000000000000, 1.000000000000000000 ) ) ;
#8135 = CARTESIAN_POINT ( 'NONE',  ( 10.00000000000000000, 0.000000000000000000, 0.000000000000000000 ) ) ;
#8136 = AXIS2_PLACEMENT_3D ( 'NONE', #7766, #12612, #1124 ) ;
#8137 = CARTESIAN_POINT ( 'NONE',  ( -10.00000000000000000, 0.000000000000000000, 0.000000000000000000 ) ) ;
#8138 = DIRECTION ( 'NONE',  ( 0.000000000000000000, -0.2756373558170062132, 0.9612616959383167847 ) ) ;
#8139 = CARTESIAN_POINT ( 'NONE',  ( 10.00000000000000000, -3.728035544476815399, 84.97818067823770605 ) ) ;
#8140 = UNCERTAINTY_MEASURE_WITH_UNIT (LENGTH_MEASURE( 1.000000000000000082E-05 ), #15750, 'distance_accuracy_value', 'NONE');
#8141 = ORIENTED_EDGE ( 'NONE', *, *, #14682, .F. ) ;
#8142 = DIRECTION ( 'NONE',  ( 0.000000000000000000, -0.9848077530122096857, 0.1736481776669207000 ) ) ;
#8143 = EDGE_CURVE ( 'NONE', #17311, #4876, #5772, .T. ) ;
#8144 = CYLINDRICAL_SURFACE ( 'NONE', #20648, 44.99999999999999289 ) ;
#8145 = ORIENTED_EDGE ( 'NONE', *, *, #3265, .T. ) ;
#8146 = DIRECTION ( 'NONE',  ( 1.000000000000000000, 0.000000000000000000, 0.000000000000000000 ) ) ;
#8147 = EDGE_LOOP ( 'NONE', ( #20742, #1420, #17739, #3319 ) ) ;
#8148 = CARTESIAN_POINT ( 'NONE',  ( -5.000000000000000000, 5.000000000000000000, 9.999999999999998224 ) ) ;
#8149 = AXIS2_PLACEMENT_3D ( 'NONE', #6985, #238, #13821 ) ;
#8150 = CARTESIAN_POINT ( 'NONE',  ( 0.000000000000000000, -87.96697768756403946, 2.410567674970269358 ) ) ;
#8151 = EDGE_LOOP ( 'NONE', ( #2324, #15446, #825, #21280 ) ) ;
#8152 = CARTESIAN_POINT ( 'NONE',  ( 10.00000000000000000, 0.000000000000000000, 0.000000000000000000 ) ) ;
#8153 = EDGE_CURVE ( 'NONE', #6675, #8963, #2588, .T. ) ;
#8154 = ORIENTED_EDGE ( 'NONE', *, *, #3439, .F. ) ;
#8155 = VERTEX_POINT ( 'NONE', #7540 ) ;
#8156 = LINE ( 'NONE', #4720, #4052 ) ;
#8157 = EDGE_CURVE ( 'NONE', #3216, #13007, #7530, .T. ) ;
#8158 = VERTEX_POINT ( 'NONE', #14272 ) ;
#8159 = DIRECTION ( 'NONE',  ( 1.000000000000000000, -0.000000000000000000, 0.000000000000000000 ) ) ;
#8160 = LINE ( 'NONE', #11463, #11477 ) ;
#8161 = DIRECTION ( 'NONE',  ( 0.000000000000000000, 0.000000000000000000, -1.000000000000000000 ) ) ;
#8162 = DIRECTION ( 'NONE',  ( -1.000000000000000000, 0.000000000000000000, 0.000000000000000000 ) ) ;
#8163 = EDGE_CURVE ( 'NONE', #4539, #10355, #11185, .T. ) ;
#8164 =( NAMED_UNIT ( * ) SI_UNIT ( $, .STERADIAN. ) SOLID_ANGLE_UNIT ( ) );
#8165 = EDGE_CURVE ( 'NONE', #3581, #9256, #14232, .T. ) ;
#8166 = CARTESIAN_POINT ( 'NONE',  ( -1.500000000000001332, 0.000000000000000000, -5.453125000000000000 ) ) ;
#8167 = LINE ( 'NONE', #14896, #20221 ) ;
#8168 = CARTESIAN_POINT ( 'NONE',  ( 0.000000000000000000, 23.62010150527335028, -84.77081340225880979 ) ) ;
#8169 = ADVANCED_FACE ( 'NONE', ( #14608 ), #822, .T. ) ;
#8170 = CARTESIAN_POINT ( 'NONE',  ( 10.00000000000000000, 0.000000000000000000, 0.000000000000000000 ) ) ;
#8171 = FACE_OUTER_BOUND ( 'NONE', #11118, .T. ) ;
#8172 = VERTEX_POINT ( 'NONE', #15098 ) ;
#8173 = ORIENTED_EDGE ( 'NONE', *, *, #6222, .F. ) ;
#8174 = EDGE_LOOP ( 'NONE', ( #18210, #2921, #19286, #16676 ) ) ;
#8175 = VERTEX_POINT ( 'NONE', #8581 ) ;
#8176 = VECTOR ( 'NONE', #5473, 1000.000000000000000 ) ;
#8177 = AXIS2_PLACEMENT_3D ( 'NONE', #5348, #8764, #20702 ) ;
#8178 = ORIENTED_EDGE ( 'NONE', *, *, #6537, .F. ) ;
#8179 = CYLINDRICAL_SURFACE ( 'NONE', #16180, 44.99999999999999289 ) ;
#8180 = VERTEX_POINT ( 'NONE', #6829 ) ;
#8181 = DIRECTION ( 'NONE',  ( -1.000000000000000000, -0.000000000000000000, -0.000000000000000000 ) ) ;
#8182 = DIRECTION ( 'NONE',  ( -1.000000000000000000, 0.000000000000000000, -0.000000000000000000 ) ) ;
#8183 = CARTESIAN_POINT ( 'NONE',  ( 10.00000000000000000, 0.000000000000000000, 0.000000000000000000 ) ) ;
#8184 = CYLINDRICAL_SURFACE ( 'NONE', #7723, 44.99999999999999289 ) ;
#8185 = FILL_AREA_STYLE_COLOUR ( '', #4123 ) ;
#8186 = DIRECTION ( 'NONE',  ( 0.000000000000000000, -0.7880107536067145757, -0.6156614753256675066 ) ) ;
#8187 = DIRECTION ( 'NONE',  ( 0.000000000000000000, 0.000000000000000000, 1.000000000000000000 ) ) ;
#8188 = ORIENTED_EDGE ( 'NONE', *, *, #20822, .T. ) ;
#8189 = CARTESIAN_POINT ( 'NONE',  ( 0.000000000000000000, -66.01871308925419157, -64.79170103523090063 ) ) ;
#8190 = ORIENTED_EDGE ( 'NONE', *, *, #9710, .F. ) ;
#8191 = ORIENTED_EDGE ( 'NONE', *, *, #11496, .T. ) ;
#8192 = CARTESIAN_POINT ( 'NONE',  ( 0.000000000000000000, -83.89484365856928605, 26.56417150042919673 ) ) ;
#8193 = ORIENTED_EDGE ( 'NONE', *, *, #11805, .F. ) ;
#8194 = DIRECTION ( 'NONE',  ( -1.000000000000000000, 0.000000000000000000, -0.000000000000000000 ) ) ;
#8195 = EDGE_LOOP ( 'NONE', ( #21561, #3504, #20638, #12105 ) ) ;
#8196 = ORIENTED_EDGE ( 'NONE', *, *, #9538, .F. ) ;
#8197 = EDGE_CURVE ( 'NONE', #10882, #20413, #14941, .T. ) ;
#8198 = DIRECTION ( 'NONE',  ( 0.000000000000000000, 0.000000000000000000, 1.000000000000000000 ) ) ;
#8199 = VERTEX_POINT ( 'NONE', #5277 ) ;
#8200 = EDGE_CURVE ( 'NONE', #12235, #378, #5426, .T. ) ;
#8201 = DIRECTION ( 'NONE',  ( -1.000000000000000000, 0.000000000000000000, 0.000000000000000000 ) ) ;
#8202 = CARTESIAN_POINT ( 'NONE',  ( 10.00000000000000000, 35.34277389771654043, -85.48288328206348297 ) ) ;
#8203 = CIRCLE ( 'NONE', #2191, 44.99999999999998579 ) ;
#8204 = DIRECTION ( 'NONE',  ( -1.000000000000000000, 0.000000000000000000, 0.000000000000000000 ) ) ;
#8205 = DIRECTION ( 'NONE',  ( -1.000000000000000000, 0.000000000000000000, 0.000000000000000000 ) ) ;
#8206 = CARTESIAN_POINT ( 'NONE',  ( 5.000000000000002665, 29.47587714451039531, 82.91666097089130005 ) ) ;
#8207 = ADVANCED_FACE ( 'NONE', ( #21841 ), #18538, .F. ) ;
#8208 = DIRECTION ( 'NONE',  ( -1.000000000000000000, -0.000000000000000000, 0.000000000000000000 ) ) ;
#8209 = DIRECTION ( 'NONE',  ( 0.000000000000000000, -0.5877852522924799095, 0.8090169943749425663 ) ) ;
#8210 = DIRECTION ( 'NONE',  ( -1.000000000000000000, 0.000000000000000000, 0.000000000000000000 ) ) ;
#8211 = AXIS2_PLACEMENT_3D ( 'NONE', #13697, #5408, #3860 ) ;
#8212 = VERTEX_POINT ( 'NONE', #15206 ) ;
#8213 = CIRCLE ( 'NONE', #12428, 88.00000000000000000 ) ;
#8214 = CARTESIAN_POINT ( 'NONE',  ( 5.000000000000002665, -83.48638250753209888, -27.82128566055197538 ) ) ;
#8215 = CARTESIAN_POINT ( 'NONE',  ( 0.000000000000000000, 60.00000000000000000, -15.00000000000000000 ) ) ;
#8216 = AXIS2_PLACEMENT_3D ( 'NONE', #20548, #1869, #17239 ) ;
#8217 = ORIENTED_EDGE ( 'NONE', *, *, #16107, .T. ) ;
#8218 = DIRECTION ( 'NONE',  ( 1.000000000000000000, 0.000000000000000000, -0.000000000000000000 ) ) ;
#8219 = EDGE_LOOP ( 'NONE', ( #16980, #14570, #5845, #16492 ) ) ;
#8220 =( NAMED_UNIT ( * ) SI_UNIT ( $, .STERADIAN. ) SOLID_ANGLE_UNIT ( ) );
#8221 = ORIENTED_EDGE ( 'NONE', *, *, #6106, .F. ) ;
#8222 = AXIS2_PLACEMENT_3D ( 'NONE', #16350, #9595, #6324 ) ;
#8224 = CIRCLE ( 'NONE', #15628, 27.49900000000000944 ) ;
#8223 = CARTESIAN_POINT ( 'NONE',  ( 10.00000000000000000, 0.000000000000000000, 0.000000000000000000 ) ) ;
#8225 = ORIENTED_EDGE ( 'NONE', *, *, #16353, .F. ) ;
#8226 = ADVANCED_FACE ( 'NONE', ( #11899 ), #13553, .T. ) ;
#8227 = VERTEX_POINT ( 'NONE', #1737 ) ;
#8228 = DIRECTION ( 'NONE',  ( 0.000000000000000000, -1.000000000000000000, 0.000000000000000000 ) ) ;
#8229 = CARTESIAN_POINT ( 'NONE',  ( 10.00000000000000000, 78.80192417387927151, 39.16958956249325752 ) ) ;
#8230 = AXIS2_PLACEMENT_3D ( 'NONE', #6795, #18502, #3355 ) ;
#8231 = ORIENTED_EDGE ( 'NONE', *, *, #19847, .F. ) ;
#8232 = LINE ( 'NONE', #13192, #2270 ) ;
#8233 = DIRECTION ( 'NONE',  ( -1.000000000000000000, -0.000000000000000000, -0.000000000000000000 ) ) ;
#8234 = DIRECTION ( 'NONE',  ( -1.000000000000000000, -0.000000000000000000, -0.000000000000000000 ) ) ;
#8235 = CARTESIAN_POINT ( 'NONE',  ( 10.00000000000000000, 0.6609040254611577847, 87.99751818016873983 ) ) ;
#8236 = CARTESIAN_POINT ( 'NONE',  ( 0.000000000000000000, -30.71797041605865175, 82.46457599186540222 ) ) ;
#8237 = CARTESIAN_POINT ( 'NONE',  ( 5.000000000000002665, -73.32282170386815778, -48.65967342042856103 ) ) ;
#8238 = AXIS2_PLACEMENT_3D ( 'NONE', #16324, #15897, #18006 ) ;
#8239 = ORIENTED_EDGE ( 'NONE', *, *, #17997, .T. ) ;
#8240 = CYLINDRICAL_SURFACE ( 'NONE', #6214, 27.49900000000000233 ) ;
#8241 = EDGE_CURVE ( 'NONE', #17170, #5244, #192, .T. ) ;
#8242 = CIRCLE ( 'NONE', #8924, 92.50100000000000477 ) ;
#8243 = CARTESIAN_POINT ( 'NONE',  ( 10.00000000000000000, 23.37352460145313060, -21.85585385440855433 ) ) ;
#8244 = ORIENTED_EDGE ( 'NONE', *, *, #4279, .T. ) ;
#8245 = CIRCLE ( 'NONE', #7897, 44.99999999999999289 ) ;
#8246 = EDGE_CURVE ( 'NONE', #13331, #15908, #8245, .T. ) ;
#8247 = FACE_OUTER_BOUND ( 'NONE', #7606, .T. ) ;
#8248 = ORIENTED_EDGE ( 'NONE', *, *, #8143, .T. ) ;
#8249 = CARTESIAN_POINT ( 'NONE',  ( -1.200000000000006617, 0.000000000000000000, -5.612499999999999822 ) ) ;
#8250 = DIRECTION ( 'NONE',  ( 0.000000000000000000, 0.000000000000000000, 1.000000000000000000 ) ) ;
#8251 = VERTEX_POINT ( 'NONE', #12007 ) ;
#8252 = FACE_OUTER_BOUND ( 'NONE', #7948, .T. ) ;
#8254 = ADVANCED_FACE ( 'NONE', ( #18749, #3603 ), #16873, .T. ) ;
#8253 = ORIENTED_EDGE ( 'NONE', *, *, #12112, .F. ) ;
#8255 = EDGE_CURVE ( 'NONE', #18016, #15663, #485, .T. ) ;
#8256 = EDGE_LOOP ( 'NONE', ( #2918, #20379, #19524, #5207 ) ) ;
#8257 = EDGE_CURVE ( 'NONE', #12158, #2019, #10351, .T. ) ;
#8258 = CARTESIAN_POINT ( 'NONE',  ( 5.000000000000000888, -30.61448696004446290, -9.314139153634542367 ) ) ;
#8259 = ORIENTED_EDGE ( 'NONE', *, *, #6393, .T. ) ;
#8260 = CARTESIAN_POINT ( 'NONE',  ( 10.00000000000000000, 19.07277123396541185, 19.80970465344755027 ) ) ;
#8261 = CIRCLE ( 'NONE', #1552, 27.49900000000000233 ) ;
#8262 = ADVANCED_FACE ( 'NONE', ( #12106 ), #18857, .T. ) ;
#8263 = CARTESIAN_POINT ( 'NONE',  ( 0.000000000000000000, -86.77540292929691645, -14.62974526292806843 ) ) ;
#8264 = DIRECTION ( 'NONE',  ( 0.000000000000000000, 0.000000000000000000, -1.000000000000000000 ) ) ;
#8265 = CARTESIAN_POINT ( 'NONE',  ( 10.00000000000000000, -30.71797041605865175, 82.46457599186540222 ) ) ;
#8266 = CARTESIAN_POINT ( 'NONE',  ( -1.500000000000001332, 0.000000000000000000, 0.000000000000000000 ) ) ;
#8267 = AXIS2_PLACEMENT_3D ( 'NONE', #1482, #8228, #13521 ) ;
#8268 = DIRECTION ( 'NONE',  ( -1.000000000000000000, -0.000000000000000000, -0.000000000000000000 ) ) ;
#8269 = CARTESIAN_POINT ( 'NONE',  ( 10.00000000000000000, -81.34229909304657724, -33.57723005635448743 ) ) ;
#8270 = CARTESIAN_POINT ( 'NONE',  ( 0.000000000000000000, -12.90282758292962662, -25.06465718894790484 ) ) ;
#8271 = EDGE_CURVE ( 'NONE', #3795, #18196, #15995, .T. ) ;
#8272 = CIRCLE ( 'NONE', #7214, 44.99999999999999289 ) ;
#8273 = DIRECTION ( 'NONE',  ( -1.000000000000000000, 0.000000000000000000, 0.000000000000000000 ) ) ;
#8274 = EDGE_CURVE ( 'NONE', #16260, #910, #7190, .T. ) ;
#8275 = EDGE_CURVE ( 'NONE', #21543, #1099, #6841, .T. ) ;
#8276 = DIRECTION ( 'NONE',  ( 0.000000000000000000, -1.000000000000000000, 0.000000000000000000 ) ) ;
#8277 = CIRCLE ( 'NONE', #4391, 32.00000000000000000 ) ;
#8278 = ORIENTED_EDGE ( 'NONE', *, *, #18911, .F. ) ;
#8279 = CARTESIAN_POINT ( 'NONE',  ( 0.000000000000000000, 0.000000000000000000, 0.000000000000000000 ) ) ;
#8280 = ORIENTED_EDGE ( 'NONE', *, *, #18483, .F. ) ;
#8281 = CIRCLE ( 'NONE', #6175, 44.99999999999999289 ) ;
#8282 = ADVANCED_FACE ( 'NONE', ( #3281 ), #10012, .F. ) ;
#8283 = VERTEX_POINT ( 'NONE', #5702 ) ;
#8284 = ORIENTED_EDGE ( 'NONE', *, *, #908, .F. ) ;
#8285 = ORIENTED_EDGE ( 'NONE', *, *, #11916, .F. ) ;
#8286 = DIRECTION ( 'NONE',  ( -1.000000000000000000, 0.000000000000000000, 0.000000000000000000 ) ) ;
#8287 = VECTOR ( 'NONE', #3020, 1000.000000000000000 ) ;
#8288 = EDGE_CURVE ( 'NONE', #16396, #9611, #12817, .T. ) ;
#8289 = ORIENTED_EDGE ( 'NONE', *, *, #5184, .F. ) ;
#8290 = DIRECTION ( 'NONE',  ( -1.000000000000000000, 0.000000000000000000, 0.000000000000000000 ) ) ;
#8291 = AXIS2_PLACEMENT_3D ( 'NONE', #21114, #13933, #2218 ) ;
#8292 = DIRECTION ( 'NONE',  ( 0.000000000000000000, 0.000000000000000000, -1.000000000000000000 ) ) ;
#8293 = FACE_OUTER_BOUND ( 'NONE', #17761, .T. ) ;
#8294 = DIRECTION ( 'NONE',  ( 0.000000000000000000, 0.8290375725550390706, 0.5591929034707507906 ) ) ;
#8295 = LINE ( 'NONE', #2776, #18252 ) ;
#8296 = AXIS2_PLACEMENT_3D ( 'NONE', #1083, #10696, #4399 ) ;
#8297 = CARTESIAN_POINT ( 'NONE',  ( 5.000000000000000000, 24.17932380791746994, -20.96092317126981186 ) ) ;
#8298 = CARTESIAN_POINT ( 'NONE',  ( 0.000000000000000000, 0.000000000000000000, 5.000000000000000000 ) ) ;
#8299 = ORIENTED_EDGE ( 'NONE', *, *, #6465, .T. ) ;
#8300 = EDGE_CURVE ( 'NONE', #7517, #10208, #19398, .T. ) ;
#8301 = DIRECTION ( 'NONE',  ( -1.000000000000000000, 0.000000000000000000, 0.000000000000000000 ) ) ;
#8302 = AXIS2_PLACEMENT_3D ( 'NONE', #19839, #14873, #21716 ) ;
#8303 = EDGE_LOOP ( 'NONE', ( #14358, #9941, #7013, #19909 ) ) ;
#8304 = CIRCLE ( 'NONE', #19958, 5.612499999999999822 ) ;
#8305 = CIRCLE ( 'NONE', #12516, 11.99999999999999822 ) ;
#8306 = EDGE_CURVE ( 'NONE', #20360, #16218, #7258, .T. ) ;
#8307 = ORIENTED_EDGE ( 'NONE', *, *, #11503, .F. ) ;
#8308 = VECTOR ( 'NONE', #11639, 1000.000000000000000 ) ;
#8309 = CARTESIAN_POINT ( 'NONE',  ( 0.000000000000000000, 0.000000000000000000, 0.000000000000000000 ) ) ;
#8310 = EDGE_LOOP ( 'NONE', ( #7269, #6695, #13080, #1763 ) ) ;
#8311 = LINE ( 'NONE', #21780, #20429 ) ;
#8312 = EDGE_LOOP ( 'NONE', ( #2320, #15064, #14993, #7074 ) ) ;
#8313 = ORIENTED_EDGE ( 'NONE', *, *, #15167, .T. ) ;
#8314 = CARTESIAN_POINT ( 'NONE',  ( 0.000000000000000000, 2.208823992044147033, 85.03123271466937183 ) ) ;
#8315 = ORIENTED_EDGE ( 'NONE', *, *, #2884, .T. ) ;
#8316 = FACE_OUTER_BOUND ( 'NONE', #14243, .T. ) ;
#8317 = DIRECTION ( 'NONE',  ( 0.000000000000000000, 0.000000000000000000, 1.000000000000000000 ) ) ;
#8318 = DIRECTION ( 'NONE',  ( -1.000000000000000000, -0.000000000000000000, -0.000000000000000000 ) ) ;
#8319 = CARTESIAN_POINT ( 'NONE',  ( 0.000000000000000000, 0.000000000000000000, 0.000000000000000000 ) ) ;
#8320 = CIRCLE ( 'NONE', #4418, 12.00000000000000178 ) ;
#8321 = AXIS2_PLACEMENT_3D ( 'NONE', #5253, #13755, #10539 ) ;
#8322 = DIRECTION ( 'NONE',  ( -1.000000000000000000, 0.000000000000000000, -0.000000000000000000 ) ) ;
#8323 = LINE ( 'NONE', #4575, #6924 ) ;
#8325 = AXIS2_PLACEMENT_3D ( 'NONE', #17693, #12172, #18922 ) ;
#8324 = CARTESIAN_POINT ( 'NONE',  ( 0.000000000000000000, -84.19736439813830486, 38.30455363800903257 ) ) ;
#8326 = ORIENTED_EDGE ( 'NONE', *, *, #13414, .F. ) ;
#8327 = ADVANCED_FACE ( 'NONE', ( #20838, #4261 ), #5816, .F. ) ;
#8328 = AXIS2_PLACEMENT_3D ( 'NONE', #13402, #13497, #8110 ) ;
#8329 = LINE ( 'NONE', #4582, #15803 ) ;
#8330 = CARTESIAN_POINT ( 'NONE',  ( 0.000000000000000000, 0.000000000000000000, 0.000000000000000000 ) ) ;
#8331 = EDGE_LOOP ( 'NONE', ( #3875, #7007, #10100, #12049 ) ) ;
#8332 = VECTOR ( 'NONE', #20462, 1000.000000000000000 ) ;
#8333 = CARTESIAN_POINT ( 'NONE',  ( 10.00000000000000000, -45.60224695560626174, 80.47900393021710386 ) ) ;
#8334 = ORIENTED_EDGE ( 'NONE', *, *, #21341, .T. ) ;
#8335 = MECHANICAL_DESIGN_GEOMETRIC_PRESENTATION_REPRESENTATION (  '', ( #17869 ), #13976 ) ;
#8336 = CIRCLE ( 'NONE', #12212, 32.00000000000000000 ) ;
#8337 = ORIENTED_EDGE ( 'NONE', *, *, #12994, .F. ) ;
#8338 = CYLINDRICAL_SURFACE ( 'NONE', #5410, 5.000000000000000888 ) ;
#8339 = VERTEX_POINT ( 'NONE', #3932 ) ;
#8340 = VERTEX_POINT ( 'NONE', #509 ) ;
#8341 = DIRECTION ( 'NONE',  ( -1.000000000000000000, -0.000000000000000000, -0.000000000000000000 ) ) ;
#8342 = EDGE_LOOP ( 'NONE', ( #8015, #4479, #4767, #17581 ) ) ;
#8343 = ORIENTED_EDGE ( 'NONE', *, *, #919, .F. ) ;
#8344 = CARTESIAN_POINT ( 'NONE',  ( 10.00000000000000000, 31.88200538760793634, -2.745493118647100772 ) ) ;
#8345 = DIRECTION ( 'NONE',  ( 0.000000000000000000, 0.000000000000000000, 1.000000000000000000 ) ) ;
#8346 = CARTESIAN_POINT ( 'NONE',  ( 6.499999999999984901, 60.00000000000001421, 0.000000000000000000 ) ) ;
#8347 = LINE ( 'NONE', #19947, #4370 ) ;
#8348 = CARTESIAN_POINT ( 'NONE',  ( 10.00000000000000000, 47.19205848891868271, -74.27590198428072199 ) ) ;
#8349 = CARTESIAN_POINT ( 'NONE',  ( -7.440711023145909486, 1.285874240517524538E-14, 104.9000000000000341 ) ) ;
#8350 = AXIS2_PLACEMENT_3D ( 'NONE', #21309, #6188, #12911 ) ;
#8351 = ORIENTED_EDGE ( 'NONE', *, *, #21534, .T. ) ;
#8352 = CARTESIAN_POINT ( 'NONE',  ( 10.00000000000000000, 51.76708072107978609, -67.49339815138442589 ) ) ;
#8353 = DIRECTION ( 'NONE',  ( 1.000000000000000000, 0.000000000000000000, 0.000000000000000000 ) ) ;
#8354 = EDGE_CURVE ( 'NONE', #10634, #4641, #731, .T. ) ;
#8355 = VERTEX_POINT ( 'NONE', #16076 ) ;
#8356 = DIRECTION ( 'NONE',  ( -1.000000000000000000, -0.000000000000000000, -0.000000000000000000 ) ) ;
#8357 = ORIENTED_EDGE ( 'NONE', *, *, #13767, .F. ) ;
#8358 =( NAMED_UNIT ( * ) SI_UNIT ( $, .STERADIAN. ) SOLID_ANGLE_UNIT ( ) );
#8359 = DIRECTION ( 'NONE',  ( -1.000000000000000000, 0.000000000000000000, 0.000000000000000000 ) ) ;
#8360 = ORIENTED_EDGE ( 'NONE', *, *, #15860, .T. ) ;
#8361 = EDGE_CURVE ( 'NONE', #9927, #16102, #20251, .T. ) ;
#8362 = DIRECTION ( 'NONE',  ( -1.000000000000000000, -0.000000000000000000, -0.000000000000000000 ) ) ;
#8363 = VECTOR ( 'NONE', #8409, 1000.000000000000000 ) ;
#8364 = ORIENTED_EDGE ( 'NONE', *, *, #19225, .F. ) ;
#8365 = ORIENTED_EDGE ( 'NONE', *, *, #19121, .F. ) ;
#8366 = CIRCLE ( 'NONE', #3785, 92.50099999999999056 ) ;
#8367 = VERTEX_POINT ( 'NONE', #14099 ) ;
#8368 = DIRECTION ( 'NONE',  ( 1.000000000000000000, 0.000000000000000000, -0.000000000000000000 ) ) ;
#8369 = AXIS2_PLACEMENT_3D ( 'NONE', #12578, #15571, #7178 ) ;
#8370 = ORIENTED_EDGE ( 'NONE', *, *, #1796, .F. ) ;
#8371 = EDGE_CURVE ( 'NONE', #5897, #3353, #19168, .T. ) ;
#8372 = DIRECTION ( 'NONE',  ( 0.000000000000000000, 1.000000000000000000, 0.000000000000000000 ) ) ;
#8373 = CARTESIAN_POINT ( 'NONE',  ( 0.000000000000000000, 0.000000000000000000, 0.000000000000000000 ) ) ;
#8374 = LINE ( 'NONE', #9913, #6787 ) ;
#8375 = CYLINDRICAL_SURFACE ( 'NONE', #9700, 45.00000000000000000 ) ;
#8376 = LINE ( 'NONE', #8053, #13510 ) ;
#8377 = CARTESIAN_POINT ( 'NONE',  ( 10.00000000000000000, -0.6609040254617754018, 87.99751818016873983 ) ) ;
#8378 = DIRECTION ( 'NONE',  ( 1.000000000000000000, -0.000000000000000000, -0.000000000000000000 ) ) ;
#8379 = CARTESIAN_POINT ( 'NONE',  ( 0.000000000000000000, 43.18649929580192293, 73.28107340219430910 ) ) ;
#8380 = AXIS2_PLACEMENT_3D ( 'NONE', #9154, #21205, #6075 ) ;
#8381 = EDGE_CURVE ( 'NONE', #5874, #10147, #13541, .T. ) ;
#8382 = DIRECTION ( 'NONE',  ( -1.000000000000000000, 0.000000000000000000, -0.000000000000000000 ) ) ;
#8383 = EDGE_CURVE ( 'NONE', #15096, #19570, #120, .T. ) ;
#8384 = CIRCLE ( 'NONE', #8741, 88.00000000000000000 ) ;
#8385 = ADVANCED_FACE ( 'NONE', ( #7140 ), #17414, .T. ) ;
#8386 = CIRCLE ( 'NONE', #9787, 92.50099999999999056 ) ;
#8388 = CIRCLE ( 'NONE', #11202, 0.2042000000000016025 ) ;
#8387 = DIRECTION ( 'NONE',  ( 1.000000000000000000, 0.000000000000000000, 0.000000000000000000 ) ) ;
#8389 = ORIENTED_EDGE ( 'NONE', *, *, #524, .T. ) ;
#8390 = EDGE_CURVE ( 'NONE', #9443, #19711, #6866, .T. ) ;
#8391 = SURFACE_SIDE_STYLE ('',( #13795 ) ) ;
#8392 = ORIENTED_EDGE ( 'NONE', *, *, #15158, .F. ) ;
#8393 = DIRECTION ( 'NONE',  ( 0.000000000000000000, 0.000000000000000000, 1.000000000000000000 ) ) ;
#8394 = ORIENTED_EDGE ( 'NONE', *, *, #16200, .T. ) ;
#8395 = ORIENTED_EDGE ( 'NONE', *, *, #18091, .T. ) ;
#8396 = ORIENTED_EDGE ( 'NONE', *, *, #15133, .F. ) ;
#8397 = ADVANCED_FACE ( 'NONE', ( #828 ), #20734, .F. ) ;
#8398 = CYLINDRICAL_SURFACE ( 'NONE', #6679, 45.00000000000000000 ) ;
#8399 = CIRCLE ( 'NONE', #14745, 88.00000000000000000 ) ;
#8400 = ORIENTED_EDGE ( 'NONE', *, *, #3439, .T. ) ;
#8401 = DIRECTION ( 'NONE',  ( 0.000000000000000000, 1.000000000000000000, -1.224646799147353207E-16 ) ) ;
#8402 = VECTOR ( 'NONE', #14947, 1000.000000000000000 ) ;
#8403 = CIRCLE ( 'NONE', #20746, 11.99999999999999822 ) ;
#8404 = CIRCLE ( 'NONE', #12630, 44.99999999999999289 ) ;
#8405 = CYLINDRICAL_SURFACE ( 'NONE', #5036, 88.00000000000000000 ) ;
#8406 = EDGE_CURVE ( 'NONE', #8251, #16392, #20607, .T. ) ;
#8407 = CYLINDRICAL_SURFACE ( 'NONE', #14209, 88.00000000000000000 ) ;
#8408 = CARTESIAN_POINT ( 'NONE',  ( 5.000000000000000000, 5.000000000000000000, 9.999999999999998224 ) ) ;
#8409 = DIRECTION ( 'NONE',  ( -1.000000000000000000, -0.000000000000000000, 0.000000000000000000 ) ) ;
#8410 = CARTESIAN_POINT ( 'NONE',  ( 10.00000000000000000, -21.65267340503310223, 89.93106657554424999 ) ) ;
#8411 = ORIENTED_EDGE ( 'NONE', *, *, #13249, .F. ) ;
#8412 = DIRECTION ( 'NONE',  ( 1.000000000000000000, 0.000000000000000000, 0.000000000000000000 ) ) ;
#8413 = EDGE_CURVE ( 'NONE', #8785, #13868, #5441, .T. ) ;
#8414 = VECTOR ( 'NONE', #19684, 1000.000000000000000 ) ;
#8415 = ORIENTED_EDGE ( 'NONE', *, *, #7824, .T. ) ;
#8416 = VECTOR ( 'NONE', #2892, 1000.000000000000000 ) ;
#8417 = AXIS2_PLACEMENT_3D ( 'NONE', #2660, #4111, #14051 ) ;
#8418 = EDGE_LOOP ( 'NONE', ( #9052, #17138, #15222, #17855 ) ) ;
#8419 = DIRECTION ( 'NONE',  ( 0.000000000000000000, 0.3420201433256630508, 0.9396926207859105373 ) ) ;
#8420 = VERTEX_POINT ( 'NONE', #619 ) ;
#8421 = CARTESIAN_POINT ( 'NONE',  ( 0.000000000000000000, 0.000000000000000000, 0.000000000000000000 ) ) ;
#8422 = ORIENTED_EDGE ( 'NONE', *, *, #5120, .T. ) ;
#8423 = VERTEX_POINT ( 'NONE', #7572 ) ;
#8424 = APPLICATION_PROTOCOL_DEFINITION ( 'draft international standard', 'automotive_design', 1998, #19692 ) ;
#8425 = EDGE_CURVE ( 'NONE', #11066, #15191, #7544, .T. ) ;
#8426 = CARTESIAN_POINT ( 'NONE',  ( 0.000000000000000000, 0.000000000000000000, 0.000000000000000000 ) ) ;
#8427 = ORIENTED_EDGE ( 'NONE', *, *, #8650, .F. ) ;
#8428 = EDGE_CURVE ( 'NONE', #16416, #5623, #6513, .T. ) ;
#8429 = CARTESIAN_POINT ( 'NONE',  ( 10.00000000000000000, 82.02147376274669455, 42.76579056660889933 ) ) ;
#8430 = AXIS2_PLACEMENT_3D ( 'NONE', #15227, #12135, #20446 ) ;
#8431 = CARTESIAN_POINT ( 'NONE',  ( 10.00000000000000000, -21.69483248597410707, -16.89761061231802586 ) ) ;
#8432 = DIRECTION ( 'NONE',  ( -1.000000000000000000, 0.000000000000000000, 0.000000000000000000 ) ) ;
#8433 = AXIS2_PLACEMENT_3D ( 'NONE', #6935, #13980, #8795 ) ;
#8434 = CARTESIAN_POINT ( 'NONE',  ( 10.00000000000000000, 27.07404830566971299, 4.815694066514526028 ) ) ;
#8435 = ADVANCED_FACE ( 'NONE', ( #5923 ), #12649, .F. ) ;
#8436 = AXIS2_PLACEMENT_3D ( 'NONE', #745, #12127, #530 ) ;
#8437 = CIRCLE ( 'NONE', #20076, 92.50100000000000477 ) ;
#8438 = AXIS2_PLACEMENT_3D ( 'NONE', #19537, #16449, #21538 ) ;
#8439 = ADVANCED_FACE ( 'NONE', ( #14752 ), #12867, .F. ) ;
#8440 = LINE ( 'NONE', #20252, #13538 ) ;
#8441 = DIRECTION ( 'NONE',  ( -1.000000000000000000, -0.000000000000000000, -0.000000000000000000 ) ) ;
#8442 = CYLINDRICAL_SURFACE ( 'NONE', #20747, 88.00000000000000000 ) ;
#8443 = VERTEX_POINT ( 'NONE', #11216 ) ;
#8444 = CARTESIAN_POINT ( 'NONE',  ( 10.00000000000000000, -90.63195040374199607, 18.50093422002390398 ) ) ;
#8445 = AXIS2_PLACEMENT_3D ( 'NONE', #1513, #6506, #19973 ) ;
#8446 = CARTESIAN_POINT ( 'NONE',  ( 5.000000000000002665, -79.38136668499713267, -37.98155635597392887 ) ) ;
#8447 = VERTEX_POINT ( 'NONE', #4366 ) ;
#8448 = CIRCLE ( 'NONE', #20776, 100.0000000000000284 ) ;
#8449 = AXIS2_PLACEMENT_3D ( 'NONE', #4945, #18426, #5162 ) ;
#8450 = LINE ( 'NONE', #18063, #7752 ) ;
#8451 = ORIENTED_EDGE ( 'NONE', *, *, #4865, .T. ) ;
#8452 = VERTEX_POINT ( 'NONE', #14423 ) ;
#8453 = CARTESIAN_POINT ( 'NONE',  ( 0.000000000000000000, 0.000000000000000000, 0.000000000000000000 ) ) ;
#8454 = ORIENTED_EDGE ( 'NONE', *, *, #14036, .T. ) ;
#8455 = ORIENTED_EDGE ( 'NONE', *, *, #10393, .F. ) ;
#8456 = CYLINDRICAL_SURFACE ( 'NONE', #7208, 27.49900000000000233 ) ;
#8457 = DIRECTION ( 'NONE',  ( -1.000000000000000000, 0.000000000000000000, 0.000000000000000000 ) ) ;
#8458 = ORIENTED_EDGE ( 'NONE', *, *, #9984, .T. ) ;
#8459 = CYLINDRICAL_SURFACE ( 'NONE', #5819, 44.99999999999999289 ) ;
#8460 = DIRECTION ( 'NONE',  ( -1.000000000000000000, 0.000000000000000000, 0.000000000000000000 ) ) ;
#8461 = CARTESIAN_POINT ( 'NONE',  ( 0.000000000000000000, -4.294029059350045863, 27.86182539015965176 ) ) ;
#8462 = DIRECTION ( 'NONE',  ( 0.000000000000000000, -0.000000000000000000, -1.000000000000000000 ) ) ;
#8463 = DIRECTION ( 'NONE',  ( -1.000000000000000000, 0.000000000000000000, -0.000000000000000000 ) ) ;
#8464 = DIRECTION ( 'NONE',  ( -1.000000000000000000, 0.000000000000000000, -0.000000000000000000 ) ) ;
#8465 = AXIS2_PLACEMENT_3D ( 'NONE', #1357, #14395, #7878 ) ;
#8466 = TOROIDAL_SURFACE ( 'NONE', #10927, 101.1000000000000512, 1.100000000000009859 ) ;
#8467 = EDGE_LOOP ( 'NONE', ( #3328, #7989, #15868, #2734 ) ) ;
#8468 = CIRCLE ( 'NONE', #7071, 45.00000000000000000 ) ;
#8469 = CARTESIAN_POINT ( 'NONE',  ( 10.00000000000000000, 51.76708072107885528, 67.49339815138510801 ) ) ;
#8470 = CARTESIAN_POINT ( 'NONE',  ( 10.00000000000000000, 77.39385041987151226, -35.28996114464630551 ) ) ;
#8471 = ORIENTED_EDGE ( 'NONE', *, *, #2768, .T. ) ;
#8472 = DIRECTION ( 'NONE',  ( 0.000000000000000000, 0.5299192642332061221, -0.8480480961564251796 ) ) ;
#8473 = ORIENTED_EDGE ( 'NONE', *, *, #6921, .T. ) ;
#8474 = CYLINDRICAL_SURFACE ( 'NONE', #19716, 88.00000000000000000 ) ;
#8475 = VERTEX_POINT ( 'NONE', #21387 ) ;
#8476 = CYLINDRICAL_SURFACE ( 'NONE', #14857, 44.99999999999999289 ) ;
#8477 = ORIENTED_EDGE ( 'NONE', *, *, #415, .F. ) ;
#8478 = ORIENTED_EDGE ( 'NONE', *, *, #9189, .F. ) ;
#8479 = ORIENTED_EDGE ( 'NONE', *, *, #13407, .T. ) ;
#8480 = CIRCLE ( 'NONE', #4248, 88.00000000000000000 ) ;
#8481 = CARTESIAN_POINT ( 'NONE',  ( 10.00000000000000000, -65.64563793391792501, -54.09103124042881916 ) ) ;
#8482 = ORIENTED_EDGE ( 'NONE', *, *, #7586, .F. ) ;
#8483 = DIRECTION ( 'NONE',  ( -1.000000000000000000, -0.000000000000000000, -0.000000000000000000 ) ) ;
#8484 = DIRECTION ( 'NONE',  ( -1.000000000000000000, -0.000000000000000000, -0.000000000000000000 ) ) ;
#8485 = DIRECTION ( 'NONE',  ( 0.000000000000000000, 0.000000000000000000, 1.000000000000000000 ) ) ;
#8486 = EDGE_CURVE ( 'NONE', #14805, #7717, #10362, .T. ) ;
#8487 = DIRECTION ( 'NONE',  ( 0.000000000000000000, 0.000000000000000000, -1.000000000000000000 ) ) ;
#8488 = CARTESIAN_POINT ( 'NONE',  ( 0.000000000000000000, -81.97107881582179800, -22.71412948308650925 ) ) ;
#8489 = LINE ( 'NONE', #11909, #11201 ) ;
#8490 = CARTESIAN_POINT ( 'NONE',  ( 10.00000000000000000, 30.61448696004464409, -9.314139153633922419 ) ) ;
#8491 = EDGE_CURVE ( 'NONE', #15070, #21459, #2706, .T. ) ;
#8492 = DIRECTION ( 'NONE',  ( -1.000000000000000000, -0.000000000000000000, -0.000000000000000000 ) ) ;
#8493 = DIRECTION ( 'NONE',  ( -1.000000000000000000, -0.000000000000000000, -0.000000000000000000 ) ) ;
#8494 = CIRCLE ( 'NONE', #18733, 27.49900000000000588 ) ;
#8495 = CARTESIAN_POINT ( 'NONE',  ( 0.000000000000000000, 21.98203405400978383, -17.64965094506522192 ) ) ;
#8496 = ORIENTED_EDGE ( 'NONE', *, *, #675, .T. ) ;
#8497 = DIRECTION ( 'NONE',  ( 0.000000000000000000, -0.7880107536067146867, -0.6156614753256676176 ) ) ;
#8498 = ORIENTED_EDGE ( 'NONE', *, *, #7707, .F. ) ;
#8499 = CARTESIAN_POINT ( 'NONE',  ( 0.000000000000000000, 0.000000000000000000, 0.000000000000000000 ) ) ;
#8500 = ORIENTED_EDGE ( 'NONE', *, *, #20674, .F. ) ;
#8501 = ORIENTED_EDGE ( 'NONE', *, *, #7840, .T. ) ;
#8502 = ORIENTED_EDGE ( 'NONE', *, *, #5716, .T. ) ;
#8503 = DIRECTION ( 'NONE',  ( 0.000000000000000000, 0.4067366430758009854, -0.9135454576426005335 ) ) ;
#8504 = EDGE_LOOP ( 'NONE', ( #4663, #3329, #21237, #2515 ) ) ;
#8505 = CARTESIAN_POINT ( 'NONE',  ( 0.000000000000000000, 72.53479564998846740, -44.42851404693280415 ) ) ;
#8506 = EDGE_CURVE ( 'NONE', #15166, #11424, #5093, .T. ) ;
#8507 = EDGE_CURVE ( 'NONE', #18557, #9877, #1555, .T. ) ;
#8508 = CARTESIAN_POINT ( 'NONE',  ( 0.000000000000000000, -9.646732466565913100, 84.51112348751846071 ) ) ;
#8509 = EDGE_CURVE ( 'NONE', #18330, #4091, #13182, .T. ) ;
#8510 = LINE ( 'NONE', #15233, #5752 ) ;
#8511 = DIRECTION ( 'NONE',  ( 1.000000000000000000, 0.000000000000000000, 0.000000000000000000 ) ) ;
#8512 = DIRECTION ( 'NONE',  ( 1.000000000000000000, 0.000000000000000000, 0.000000000000000000 ) ) ;
#8513 = CARTESIAN_POINT ( 'NONE',  ( 10.00000000000000000, 41.21966518005955038, 82.80926399530301296 ) ) ;
#8514 = DIRECTION ( 'NONE',  ( 0.000000000000000000, 0.000000000000000000, 1.000000000000000000 ) ) ;
#8515 = ORIENTED_EDGE ( 'NONE', *, *, #8835, .T. ) ;
#8516 = CYLINDRICAL_SURFACE ( 'NONE', #9029, 45.00000000000000000 ) ;
#8517 = ADVANCED_FACE ( 'NONE', ( #12755 ), #3321, .T. ) ;
#8518 = ORIENTED_EDGE ( 'NONE', *, *, #9163, .F. ) ;
#8519 = ORIENTED_EDGE ( 'NONE', *, *, #16501, .T. ) ;
#8520 = ADVANCED_FACE ( 'NONE', ( #1280 ), #8960, .T. ) ;
#8521 = FACE_OUTER_BOUND ( 'NONE', #7334, .T. ) ;
#8522 = ORIENTED_EDGE ( 'NONE', *, *, #3411, .F. ) ;
#8523 = DIRECTION ( 'NONE',  ( 0.000000000000000000, 0.000000000000000000, 1.000000000000000000 ) ) ;
#8524 = VERTEX_POINT ( 'NONE', #1161 ) ;
#8525 = ORIENTED_EDGE ( 'NONE', *, *, #1112, .T. ) ;
#8526 = CARTESIAN_POINT ( 'NONE',  ( 10.00000000000000000, 69.74988376404020585, 53.65588238863360715 ) ) ;
#8527 = EDGE_CURVE ( 'NONE', #15310, #3214, #16721, .T. ) ;
#8528 = ORIENTED_EDGE ( 'NONE', *, *, #517, .T. ) ;
#8529 = EDGE_CURVE ( 'NONE', #11017, #11720, #14953, .T. ) ;
#8530 = DIRECTION ( 'NONE',  ( 1.000000000000000000, 0.000000000000000000, 0.000000000000000000 ) ) ;
#8531 = EDGE_CURVE ( 'NONE', #19278, #2087, #138, .T. ) ;
#8532 = DIRECTION ( 'NONE',  ( 0.000000000000000000, 1.000000000000000000, 0.000000000000000000 ) ) ;
#8533 = DIRECTION ( 'NONE',  ( 0.000000000000000000, 0.000000000000000000, -1.000000000000000000 ) ) ;
#8534 = AXIS2_PLACEMENT_3D ( 'NONE', #19184, #12014, #18868 ) ;
#8535 = CARTESIAN_POINT ( 'NONE',  ( -1.500000000000000000, -7.000000000000000000, 5.000000000000000000 ) ) ;
#8536 = FACE_OUTER_BOUND ( 'NONE', #6147, .T. ) ;
#8537 = CARTESIAN_POINT ( 'NONE',  ( 10.00000000000000000, 35.18804927320642406, -80.65854690202642985 ) ) ;
#8538 = DIRECTION ( 'NONE',  ( 1.000000000000000000, 0.000000000000000000, 0.000000000000000000 ) ) ;
#8539 = EDGE_LOOP ( 'NONE', ( #10493, #12104, #5827, #8239 ) ) ;
#8540 = AXIS2_PLACEMENT_3D ( 'NONE', #14891, #21627, #8264 ) ;
#8541 = ADVANCED_FACE ( 'NONE', ( #19724 ), #8129, .T. ) ;
#8542 = ADVANCED_FACE ( 'NONE', ( #9648 ), #18847, .T. ) ;
#8543 = FACE_OUTER_BOUND ( 'NONE', #12394, .T. ) ;
#8544 = DIRECTION ( 'NONE',  ( 1.000000000000000000, 0.000000000000000000, 0.000000000000000000 ) ) ;
#8545 = VERTEX_POINT ( 'NONE', #4691 ) ;
#8546 = DIRECTION ( 'NONE',  ( -1.000000000000000000, 0.000000000000000000, 0.000000000000000000 ) ) ;
#8547 = ORIENTED_EDGE ( 'NONE', *, *, #7302, .T. ) ;
#8548 = EDGE_CURVE ( 'NONE', #13890, #4009, #15666, .T. ) ;
#8549 = ORIENTED_EDGE ( 'NONE', *, *, #1205, .F. ) ;
#8550 = DIRECTION ( 'NONE',  ( 1.000000000000000000, 0.000000000000000000, 0.000000000000000000 ) ) ;
#8551 = AXIS2_PLACEMENT_3D ( 'NONE', #2442, #10507, #360 ) ;
#8552 = ORIENTED_EDGE ( 'NONE', *, *, #4369, .F. ) ;
#8553 = VERTEX_POINT ( 'NONE', #13188 ) ;
#8554 = CARTESIAN_POINT ( 'NONE',  ( 10.00000000000000000, 19.29292659244005037, 25.53004080487768235 ) ) ;
#8555 = DIRECTION ( 'NONE',  ( -1.000000000000000000, 0.000000000000000000, 0.000000000000000000 ) ) ;
#8556 = ORIENTED_EDGE ( 'NONE', *, *, #7331, .F. ) ;
#8557 = EDGE_CURVE ( 'NONE', #20994, #17054, #11429, .T. ) ;
#8558 = DIRECTION ( 'NONE',  ( 0.000000000000000000, 0.000000000000000000, 1.000000000000000000 ) ) ;
#8559 = CARTESIAN_POINT ( 'NONE',  ( 0.000000000000000000, -84.12297548659712731, 32.40974838672912028 ) ) ;
#8560 = DIRECTION ( 'NONE',  ( 0.000000000000000000, 0.2079116908177532363, 0.9781476007338069101 ) ) ;
#8561 = CARTESIAN_POINT ( 'NONE',  ( 10.00000000000000000, -70.37753541435978377, 60.02863908169610596 ) ) ;
#8562 = AXIS2_PLACEMENT_3D ( 'NONE', #18760, #17214, #7059 ) ;
#8563 = LINE ( 'NONE', #21824, #6137 ) ;
#8564 = DIRECTION ( 'NONE',  ( -0.000000000000000000, -0.000000000000000000, -1.000000000000000000 ) ) ;
#8565 = EDGE_LOOP ( 'NONE', ( #19499, #9944, #12134, #4644 ) ) ;
#8566 = DIRECTION ( 'NONE',  ( 0.000000000000000000, 0.000000000000000000, 1.000000000000000000 ) ) ;
#8567 = CARTESIAN_POINT ( 'NONE',  ( -2.000000000000000000, 67.00000000000000000, 9.999999999999998224 ) ) ;
#8568 = VERTEX_POINT ( 'NONE', #5136 ) ;
#8569 = FACE_OUTER_BOUND ( 'NONE', #15631, .T. ) ;
#8570 = VERTEX_POINT ( 'NONE', #4925 ) ;
#8571 = CIRCLE ( 'NONE', #17389, 44.99999999999998579 ) ;
#8572 = CYLINDRICAL_SURFACE ( 'NONE', #18694, 44.99999999999999289 ) ;
#8573 = LINE ( 'NONE', #8888, #1382 ) ;
#8574 = EDGE_LOOP ( 'NONE', ( #1434, #10718, #9356, #10934 ) ) ;
#8575 = CIRCLE ( 'NONE', #20921, 88.00000000000000000 ) ;
#8576 = EDGE_CURVE ( 'NONE', #10685, #17273, #17787, .T. ) ;
#8577 = DIRECTION ( 'NONE',  ( 0.000000000000000000, 0.000000000000000000, 1.000000000000000000 ) ) ;
#8578 = ORIENTED_EDGE ( 'NONE', *, *, #10642, .F. ) ;
#8579 = ORIENTED_EDGE ( 'NONE', *, *, #10813, .T. ) ;
#8580 = ORIENTED_EDGE ( 'NONE', *, *, #20447, .T. ) ;
#8581 = CARTESIAN_POINT ( 'NONE',  ( 10.00000000000000000, -7.619321854369379032, -26.42235673590698397 ) ) ;
#8582 = ORIENTED_EDGE ( 'NONE', *, *, #12290, .T. ) ;
#8583 = DIRECTION ( 'NONE',  ( 1.000000000000000000, 0.000000000000000000, 0.000000000000000000 ) ) ;
#8584 = AXIS2_PLACEMENT_3D ( 'NONE', #20198, #11466, #16441 ) ;
#8585 = CARTESIAN_POINT ( 'NONE',  ( 10.00000000000000000, -2.208823992044743445, 85.03123271466935762 ) ) ;
#8586 = CARTESIAN_POINT ( 'NONE',  ( 0.000000000000000000, 79.66702613806732813, 29.80527447819576636 ) ) ;
#8587 = DIRECTION ( 'NONE',  ( -1.000000000000000000, 0.000000000000000000, -0.000000000000000000 ) ) ;
#8588 = DIRECTION ( 'NONE',  ( 0.000000000000000000, 0.9945218953682729568, 0.1045284632676570374 ) ) ;
#8589 = CIRCLE ( 'NONE', #20933, 115.1000000000000227 ) ;
#8590 = DIRECTION ( 'NONE',  ( -1.000000000000000000, 0.000000000000000000, 0.000000000000000000 ) ) ;
#8591 = CARTESIAN_POINT ( 'NONE',  ( 0.000000000000000000, 6.063030049135076816, 31.42037024962127134 ) ) ;
#8592 = VECTOR ( 'NONE', #7046, 1000.000000000000000 ) ;
#8593 = CARTESIAN_POINT ( 'NONE',  ( 10.00000000000000000, -18.31866948046747723, -26.23788002993743262 ) ) ;
#8594 = CARTESIAN_POINT ( 'NONE',  ( 0.000000000000000000, -71.33759994381919967, -58.88447872959059737 ) ) ;
#8595 = CARTESIAN_POINT ( 'NONE',  ( 1.199999999999992628, 0.000000000000000000, 0.000000000000000000 ) ) ;
#8596 = VERTEX_POINT ( 'NONE', #13419 ) ;
#8597 = AXIS2_PLACEMENT_3D ( 'NONE', #13782, #20624, #20522 ) ;
#8598 = LINE ( 'NONE', #13473, #10533 ) ;
#8599 = ORIENTED_EDGE ( 'NONE', *, *, #16589, .F. ) ;
#8600 = DIRECTION ( 'NONE',  ( 1.000000000000000000, -0.000000000000000000, -0.000000000000000000 ) ) ;
#8601 = ORIENTED_EDGE ( 'NONE', *, *, #7014, .T. ) ;
#8602 = CIRCLE ( 'NONE', #18494, 44.99999999999999289 ) ;
#8603 = EDGE_LOOP ( 'NONE', ( #13380, #873, #13303, #18060 ) ) ;
#8604 = AXIS2_PLACEMENT_3D ( 'NONE', #6040, #11319, #14529 ) ;
#8605 = ORIENTED_EDGE ( 'NONE', *, *, #3952, .T. ) ;
#8606 = DIRECTION ( 'NONE',  ( 0.000000000000000000, 0.000000000000000000, 1.000000000000000000 ) ) ;
#8607 = ORIENTED_EDGE ( 'NONE', *, *, #13405, .T. ) ;
#8608 = DIRECTION ( 'NONE',  ( 0.000000000000000000, 1.000000000000000000, 0.000000000000000000 ) ) ;
#8609 = DIRECTION ( 'NONE',  ( 0.000000000000000000, 0.000000000000000000, 1.000000000000000000 ) ) ;
#8610 = VECTOR ( 'NONE', #1824, 1000.000000000000000 ) ;
#8611 = LINE ( 'NONE', #13585, #5405 ) ;
#8612 = CARTESIAN_POINT ( 'NONE',  ( 0.000000000000000000, 0.000000000000000000, 0.000000000000000000 ) ) ;
#8613 = CARTESIAN_POINT ( 'NONE',  ( -7.500000000000000000, 0.000000000000000000, -3.000000000000000000 ) ) ;
#8614 = CARTESIAN_POINT ( 'NONE',  ( 0.000000000000000000, 0.000000000000000000, 0.000000000000000000 ) ) ;
#8615 = DIRECTION ( 'NONE',  ( 0.000000000000000000, 0.000000000000000000, -1.000000000000000000 ) ) ;
#8616 = CIRCLE ( 'NONE', #15680, 5.000000000000000000 ) ;
#8617 = EDGE_LOOP ( 'NONE', ( #3580, #11335, #14181, #11240 ) ) ;
#8618 = PRODUCT_DEFINITION_SHAPE ( 'NONE', 'NONE',  #21860 ) ;
#8619 = AXIS2_PLACEMENT_3D ( 'NONE', #13960, #705, #8872 ) ;
#8620 = DIRECTION ( 'NONE',  ( -1.000000000000000000, -0.000000000000000000, -0.000000000000000000 ) ) ;
#8621 = ADVANCED_FACE ( 'NONE', ( #1595 ), #8456, .T. ) ;
#8622 = VERTEX_POINT ( 'NONE', #8554 ) ;
#8623 = ORIENTED_EDGE ( 'NONE', *, *, #5910, .T. ) ;
#8624 = CARTESIAN_POINT ( 'NONE',  ( 10.00000000000000000, 27.00677879429026618, 80.65868421664441712 ) ) ;
#8625 = AXIS2_PLACEMENT_3D ( 'NONE', #10374, #20870, #12144 ) ;
#8626 = ORIENTED_EDGE ( 'NONE', *, *, #13126, .F. ) ;
#8627 = ORIENTED_EDGE ( 'NONE', *, *, #17266, .F. ) ;
#8628 = EDGE_CURVE ( 'NONE', #12477, #11073, #19544, .T. ) ;
#8629 = AXIS2_PLACEMENT_3D ( 'NONE', #382, #7020, #7121 ) ;
#8630 = DIRECTION ( 'NONE',  ( -1.000000000000000000, -0.000000000000000000, -0.000000000000000000 ) ) ;
#8631 = ORIENTED_EDGE ( 'NONE', *, *, #1892, .F. ) ;
#8632 = VECTOR ( 'NONE', #13117, 1000.000000000000114 ) ;
#8633 = FACE_OUTER_BOUND ( 'NONE', #14120, .T. ) ;
#8634 = ADVANCED_FACE ( 'NONE', ( #11981 ), #7017, .T. ) ;
#8635 = DIRECTION ( 'NONE',  ( 0.000000000000000000, 0.000000000000000000, 1.000000000000000000 ) ) ;
#8636 = CARTESIAN_POINT ( 'NONE',  ( 0.000000000000000000, 0.000000000000000000, 0.000000000000000000 ) ) ;
#8637 = DIRECTION ( 'NONE',  ( 0.000000000000000000, 0.9945218953682729568, 0.1045284632676570374 ) ) ;
#8638 = CARTESIAN_POINT ( 'NONE',  ( 10.00000000000000000, -10.41137886060045226, -91.91321010181856366 ) ) ;
#8639 = DIRECTION ( 'NONE',  ( -1.000000000000000000, -0.000000000000000000, -0.000000000000000000 ) ) ;
#8640 = FACE_OUTER_BOUND ( 'NONE', #9002, .T. ) ;
#8641 = CIRCLE ( 'NONE', #5830, 5.000000000000000000 ) ;
#8642 = AXIS2_PLACEMENT_3D ( 'NONE', #8063, #16776, #11699 ) ;
#8643 = ORIENTED_EDGE ( 'NONE', *, *, #7270, .T. ) ;
#8644 = AXIS2_PLACEMENT_3D ( 'NONE', #15643, #8587, #15318 ) ;
#8645 = ADVANCED_FACE ( 'NONE', ( #21815 ), #499, .T. ) ;
#8646 = EDGE_CURVE ( 'NONE', #6638, #7563, #6800, .T. ) ;
#8647 = EDGE_CURVE ( 'NONE', #13868, #8785, #21313, .T. ) ;
#8648 = AXIS2_PLACEMENT_3D ( 'NONE', #3720, #10342, #17208 ) ;
#8649 = DIRECTION ( 'NONE',  ( -1.000000000000000000, -0.000000000000000000, 0.000000000000000000 ) ) ;
#8650 = EDGE_CURVE ( 'NONE', #14884, #14755, #18617, .T. ) ;
#8651 = CARTESIAN_POINT ( 'NONE',  ( 0.000000000000000000, 0.000000000000000000, 0.000000000000000000 ) ) ;
#8652 = ORIENTED_EDGE ( 'NONE', *, *, #17949, .T. ) ;
#8653 = VECTOR ( 'NONE', #13305, 1000.000000000000000 ) ;
#8654 = DIRECTION ( 'NONE',  ( -1.000000000000000000, 0.000000000000000000, 0.000000000000000000 ) ) ;
#8655 = ORIENTED_EDGE ( 'NONE', *, *, #12813, .T. ) ;
#8656 = ORIENTED_EDGE ( 'NONE', *, *, #14887, .T. ) ;
#8657 = DIRECTION ( 'NONE',  ( 0.000000000000000000, -0.4067366430757887175, -0.9135454576426059736 ) ) ;
#8658 = ORIENTED_EDGE ( 'NONE', *, *, #8413, .F. ) ;
#8659 = AXIS2_PLACEMENT_3D ( 'NONE', #18198, #8353, #19743 ) ;
#8660 = ORIENTED_EDGE ( 'NONE', *, *, #4747, .T. ) ;
#8661 = DIRECTION ( 'NONE',  ( 0.000000000000000000, 0.000000000000000000, 1.000000000000000000 ) ) ;
#8662 = DIRECTION ( 'NONE',  ( -1.000000000000000000, -0.000000000000000000, 0.000000000000000000 ) ) ;
#8663 = CIRCLE ( 'NONE', #17848, 88.00000000000000000 ) ;
#8664 = AXIS2_PLACEMENT_3D ( 'NONE', #17510, #16051, #5678 ) ;
#8665 = EDGE_CURVE ( 'NONE', #18379, #13984, #4728, .T. ) ;
#8666 = CIRCLE ( 'NONE', #211, 44.99999999999999289 ) ;
#8667 = DIRECTION ( 'NONE',  ( 1.000000000000000000, 0.000000000000000000, 0.000000000000000000 ) ) ;
#8668 = CARTESIAN_POINT ( 'NONE',  ( 10.00000000000000000, 78.80192417387979731, -39.16958956249220591 ) ) ;
#8669 = LINE ( 'NONE', #13639, #5500 ) ;
#8670 = CARTESIAN_POINT ( 'NONE',  ( 0.000000000000000000, 0.000000000000000000, 0.000000000000000000 ) ) ;
#8671 = DIRECTION ( 'NONE',  ( -1.000000000000000000, -0.000000000000000000, -0.000000000000000000 ) ) ;
#8672 = EDGE_CURVE ( 'NONE', #11073, #1127, #5247, .T. ) ;
#8673 = CARTESIAN_POINT ( 'NONE',  ( 10.00000000000000000, -23.37352460145297783, 21.85585385440871775 ) ) ;
#8674 = ORIENTED_EDGE ( 'NONE', *, *, #3940, .F. ) ;
#8675 = ADVANCED_FACE ( 'NONE', ( #10214 ), #267, .F. ) ;
#8676 = DIRECTION ( 'NONE',  ( 1.000000000000000000, 0.000000000000000000, 0.000000000000000000 ) ) ;
#8677 = DIRECTION ( 'NONE',  ( 0.000000000000000000, 0.06975647374412555224, -0.9975640502598241977 ) ) ;
#8678 = ORIENTED_EDGE ( 'NONE', *, *, #10714, .F. ) ;
#8679 = AXIS2_PLACEMENT_3D ( 'NONE', #6816, #784, #3593 ) ;
#8680 = AXIS2_PLACEMENT_3D ( 'NONE', #7457, #813, #20927 ) ;
#8681 = AXIS2_PLACEMENT_3D ( 'NONE', #34, #10294, #11849 ) ;
#8682 = CARTESIAN_POINT ( 'NONE',  ( 0.000000000000000000, 0.000000000000000000, 0.000000000000000000 ) ) ;
#8683 = AXIS2_PLACEMENT_3D ( 'NONE', #3778, #2127, #14150 ) ;
#8684 = ORIENTED_EDGE ( 'NONE', *, *, #19758, .T. ) ;
#8685 = EDGE_CURVE ( 'NONE', #8843, #19024, #6909, .T. ) ;
#8686 = LINE ( 'NONE', #11568, #11266 ) ;
#8687 = CYLINDRICAL_SURFACE ( 'NONE', #13391, 44.99999999999998579 ) ;
#8688 = ORIENTED_EDGE ( 'NONE', *, *, #17886, .T. ) ;
#8689 = ORIENTED_EDGE ( 'NONE', *, *, #4573, .F. ) ;
#8690 = ORIENTED_EDGE ( 'NONE', *, *, #20898, .F. ) ;
#8691 = VERTEX_POINT ( 'NONE', #13633 ) ;
#8692 = CARTESIAN_POINT ( 'NONE',  ( 7.440711023145912151, 0.000000000000000000, 0.000000000000000000 ) ) ;
#8693 = ORIENTED_EDGE ( 'NONE', *, *, #10150, .F. ) ;
#8694 =( REPRESENTATION_RELATIONSHIP ('NONE','NONE', #2177, #16445 ) REPRESENTATION_RELATIONSHIP_WITH_TRANSFORMATION ( #6672 )SHAPE_REPRESENTATION_RELATIONSHIP( ) );
#8695 = DIRECTION ( 'NONE',  ( 0.000000000000000000, -0.8660254037844327124, -0.5000000000000103251 ) ) ;
#8696 = CARTESIAN_POINT ( 'NONE',  ( 5.000000000000002665, 11.59241532900744787, -87.23311244498727035 ) ) ;
#8697 = FACE_OUTER_BOUND ( 'NONE', #9337, .T. ) ;
#8698 = AXIS2_PLACEMENT_3D ( 'NONE', #20661, #5527, #19012 ) ;
#8699 = CARTESIAN_POINT ( 'NONE',  ( 0.000000000000000000, 84.33453774737657227, 11.08490790852157559 ) ) ;
#8700 = EDGE_CURVE ( 'NONE', #11814, #8596, #857, .T. ) ;
#8701 = DIRECTION ( 'NONE',  ( 0.000000000000000000, 0.000000000000000000, -1.000000000000000000 ) ) ;
#8702 = CIRCLE ( 'NONE', #1652, 32.00000000000000000 ) ;
#8703 = CIRCLE ( 'NONE', #928, 6.887500000000022382 ) ;
#8704 = FACE_OUTER_BOUND ( 'NONE', #8310, .T. ) ;
#8705 = CARTESIAN_POINT ( 'NONE',  ( 10.00000000000000000, -23.10190250628894404, 89.56973317806591695 ) ) ;
#8706 = DIRECTION ( 'NONE',  ( -1.000000000000000000, -0.000000000000000000, -0.000000000000000000 ) ) ;
#8707 = ADVANCED_FACE ( 'NONE', ( #12080 ), #17062, .F. ) ;
#8708 = VERTEX_POINT ( 'NONE', #6589 ) ;
#8709 = ADVANCED_FACE ( 'NONE', ( #18831 ), #18505, .T. ) ;
#8710 = LINE ( 'NONE', #18444, #5996 ) ;
#8711 = CARTESIAN_POINT ( 'NONE',  ( 10.00000000000000000, 0.000000000000000000, 0.000000000000000000 ) ) ;
#8712 = DIRECTION ( 'NONE',  ( -1.000000000000000000, 0.000000000000000000, -0.000000000000000000 ) ) ;
#8713 = ORIENTED_EDGE ( 'NONE', *, *, #12604, .T. ) ;
#8714 = AXIS2_PLACEMENT_3D ( 'NONE', #8614, #13589, #17243 ) ;
#8715 = CARTESIAN_POINT ( 'NONE',  ( -140.0000507999999968, 0.000000000000000000, 0.000000000000000000 ) ) ;
#8716 = VECTOR ( 'NONE', #2084, 1000.000000000000000 ) ;
#8717 = EDGE_LOOP ( 'NONE', ( #16644, #8658 ) ) ;
#8718 = DIRECTION ( 'NONE',  ( 0.000000000000000000, 0.000000000000000000, 1.000000000000000000 ) ) ;
#8719 = ORIENTED_EDGE ( 'NONE', *, *, #1270, .T. ) ;
#8720 = VERTEX_POINT ( 'NONE', #3250 ) ;
#8721 = EDGE_LOOP ( 'NONE', ( #8188, #18172, #7643, #7367 ) ) ;
#8722 = CARTESIAN_POINT ( 'NONE',  ( 10.00000000000000000, 71.72924546250010280, -45.71766382684594276 ) ) ;
#8723 = EDGE_LOOP ( 'NONE', ( #17316, #18211, #6256, #16096 ) ) ;
#8724 = DIRECTION ( 'NONE',  ( -1.000000000000000000, -0.000000000000000000, 0.000000000000000000 ) ) ;
#8725 = DIRECTION ( 'NONE',  ( -1.000000000000000000, -0.000000000000000000, -0.000000000000000000 ) ) ;
#8726 = LINE ( 'NONE', #18890, #18099 ) ;
#8727 = PRODUCT_DEFINITION_CONTEXT ( 'detailed design', #7281, 'design' ) ;
#8728 = AXIS2_PLACEMENT_3D ( 'NONE', #18227, #16448, #6306 ) ;
#8729 = FACE_OUTER_BOUND ( 'NONE', #20018, .T. ) ;
#8730 = LINE ( 'NONE', #343, #5543 ) ;
#8731 = LINE ( 'NONE', #3968, #12156 ) ;
#8732 = CARTESIAN_POINT ( 'NONE',  ( 0.000000000000000000, 77.39385041987100067, 35.28996114464738554 ) ) ;
#8733 = DIRECTION ( 'NONE',  ( 1.000000000000000000, 0.000000000000000000, 0.000000000000000000 ) ) ;
#8734 = EDGE_LOOP ( 'NONE', ( #19798, #18935, #17815, #14604 ) ) ;
#8735 = DIRECTION ( 'NONE',  ( 0.000000000000000000, 0.000000000000000000, 1.000000000000000000 ) ) ;
#8736 = ORIENTED_EDGE ( 'NONE', *, *, #7319, .T. ) ;
#8737 = VERTEX_POINT ( 'NONE', #7341 ) ;
#8738 = AXIS2_PLACEMENT_3D ( 'NONE', #12468, #761, #4082 ) ;
#8739 = CARTESIAN_POINT ( 'NONE',  ( 10.00000000000000000, 41.21966518006070146, -82.80926399530243032 ) ) ;
#8740 = ORIENTED_EDGE ( 'NONE', *, *, #14819, .F. ) ;
#8741 = AXIS2_PLACEMENT_3D ( 'NONE', #8682, #13863, #11886 ) ;
#8742 = EDGE_LOOP ( 'NONE', ( #20910, #6498, #11510, #15033 ) ) ;
#8743 = AXIS2_PLACEMENT_3D ( 'NONE', #7939, #6412, #9366 ) ;
#8744 = DIRECTION ( 'NONE',  ( 0.000000000000000000, 0.000000000000000000, 1.000000000000000000 ) ) ;
#8745 = ORIENTED_EDGE ( 'NONE', *, *, #21533, .T. ) ;
#8746 = FACE_OUTER_BOUND ( 'NONE', #12704, .T. ) ;
#8747 = DIRECTION ( 'NONE',  ( 0.000000000000000000, 0.000000000000000000, -1.000000000000000000 ) ) ;
#8748 = LINE ( 'NONE', #20475, #16875 ) ;
#8749 = EDGE_CURVE ( 'NONE', #3486, #1974, #14256, .T. ) ;
#8750 = DIRECTION ( 'NONE',  ( 1.000000000000000000, -0.000000000000000000, 0.000000000000000000 ) ) ;
#8751 = CARTESIAN_POINT ( 'NONE',  ( 10.00000000000000000, 33.95793648385814123, 86.04239391578002483 ) ) ;
#8752 = DIRECTION ( 'NONE',  ( 1.000000000000000000, 0.000000000000000000, 0.000000000000000000 ) ) ;
#8753 = DIRECTION ( 'NONE',  ( 0.000000000000000000, 0.000000000000000000, 1.000000000000000000 ) ) ;
#8754 = CIRCLE ( 'NONE', #11567, 92.50100000000000477 ) ;
#8755 = CIRCLE ( 'NONE', #18298, 88.00000000000000000 ) ;
#8756 = ORIENTED_EDGE ( 'NONE', *, *, #4300, .T. ) ;
#8757 = VECTOR ( 'NONE', #18278, 1000.000000000000000 ) ;
#8758 = ADVANCED_FACE ( 'NONE', ( #5898 ), #2242, .T. ) ;
#8759 = DIRECTION ( 'NONE',  ( 0.000000000000000000, 0.9945218953682736229, -0.1045284632676503761 ) ) ;
#8760 = DIRECTION ( 'NONE',  ( 0.000000000000000000, 0.000000000000000000, -1.000000000000000000 ) ) ;
#8761 = ORIENTED_EDGE ( 'NONE', *, *, #3783, .T. ) ;
#8762 = CARTESIAN_POINT ( 'NONE',  ( 0.000000000000000000, 25.17124263951009411, 12.69364185792227495 ) ) ;
#8763 = ORIENTED_EDGE ( 'NONE', *, *, #16924, .T. ) ;
#8764 = DIRECTION ( 'NONE',  ( 0.000000000000000000, 0.000000000000000000, 1.000000000000000000 ) ) ;
#8765 = AXIS2_PLACEMENT_3D ( 'NONE', #17791, #14477, #17583 ) ;
#8766 = DIRECTION ( 'NONE',  ( -1.000000000000000000, 0.000000000000000000, -0.000000000000000000 ) ) ;
#8767 = ORIENTED_EDGE ( 'NONE', *, *, #3418, .T. ) ;
#8768 = VECTOR ( 'NONE', #18770, 1000.000000000000000 ) ;
#8769 = EDGE_LOOP ( 'NONE', ( #21427, #9618, #21346, #10382 ) ) ;
#8770 = CARTESIAN_POINT ( 'NONE',  ( -123.0000000000000000, 1.506315562951244531E-14, -3.000000000000000000 ) ) ;
#8771 = AXIS2_PLACEMENT_3D ( 'NONE', #14930, #3002, #16368 ) ;
#8772 = LINE ( 'NONE', #10534, #2909 ) ;
#8773 = CIRCLE ( 'NONE', #1714, 88.00000000000000000 ) ;
#8774 = LINE ( 'NONE', #5143, #5474 ) ;
#8775 = CARTESIAN_POINT ( 'NONE',  ( 0.000000000000000000, 83.35585896458643163, -16.94078559807864792 ) ) ;
#8776 = EDGE_CURVE ( 'NONE', #2079, #7213, #21326, .T. ) ;
#8777 = EDGE_CURVE ( 'NONE', #9461, #2562, #12855, .T. ) ;
#8778 = LINE ( 'NONE', #15516, #20666 ) ;
#8779 = EDGE_CURVE ( 'NONE', #19086, #3139, #14276, .T. ) ;
#8780 = FACE_OUTER_BOUND ( 'NONE', #13872, .T. ) ;
#8781 = DIRECTION ( 'NONE',  ( -1.000000000000000000, 0.000000000000000000, 0.000000000000000000 ) ) ;
#8782 = CARTESIAN_POINT ( 'NONE',  ( 10.00000000000000000, -21.31452625070983231, 82.34610137166113475 ) ) ;
#8783 = EDGE_CURVE ( 'NONE', #1843, #20663, #16738, .T. ) ;
#8784 = CIRCLE ( 'NONE', #15483, 92.50100000000000477 ) ;
#8785 = VERTEX_POINT ( 'NONE', #20911 ) ;
#8786 = CARTESIAN_POINT ( 'NONE',  ( 8.000000000000007105, 0.000000000000000000, -104.9000000000000341 ) ) ;
#8787 = AXIS2_PLACEMENT_3D ( 'NONE', #7495, #5954, #4398 ) ;
#8788 = CIRCLE ( 'NONE', #11252, 11.99999999999999645 ) ;
#8789 = ORIENTED_EDGE ( 'NONE', *, *, #6942, .F. ) ;
#8790 = AXIS2_PLACEMENT_3D ( 'NONE', #11336, #14547, #9668 ) ;
#8791 = CYLINDRICAL_SURFACE ( 'NONE', #17912, 92.50100000000000477 ) ;
#8792 = EDGE_CURVE ( 'NONE', #752, #12349, #14972, .T. ) ;
#8793 = EDGE_LOOP ( 'NONE', ( #4830, #21812, #9293, #20754 ) ) ;
#8794 = CARTESIAN_POINT ( 'NONE',  ( 10.00000000000000000, 0.000000000000000000, 0.000000000000000000 ) ) ;
#8795 = DIRECTION ( 'NONE',  ( 0.000000000000000000, 0.000000000000000000, 1.000000000000000000 ) ) ;
#8796 = ORIENTED_EDGE ( 'NONE', *, *, #11255, .T. ) ;
#8797 =( LENGTH_UNIT ( ) NAMED_UNIT ( * ) SI_UNIT ( .MILLI., .METRE. ) );
#8798 = EDGE_CURVE ( 'NONE', #17227, #9309, #9314, .T. ) ;
#8799 = ORIENTED_EDGE ( 'NONE', *, *, #4517, .T. ) ;
#8800 = ORIENTED_EDGE ( 'NONE', *, *, #2532, .T. ) ;
#8801 = ORIENTED_EDGE ( 'NONE', *, *, #20622, .F. ) ;
#8802 = DIRECTION ( 'NONE',  ( -1.000000000000000000, -0.000000000000000000, 0.000000000000000000 ) ) ;
#8803 = ORIENTED_EDGE ( 'NONE', *, *, #3844, .F. ) ;
#8804 = DIRECTION ( 'NONE',  ( 0.000000000000000000, -0.8987940462991619306, -0.4383711467890878399 ) ) ;
#8805 = AXIS2_PLACEMENT_3D ( 'NONE', #5899, #17826, #19587 ) ;
#8806 = CARTESIAN_POINT ( 'NONE',  ( 0.000000000000000000, -23.62010150527165919, -84.77081340225927875 ) ) ;
#8807 = DIRECTION ( 'NONE',  ( 0.000000000000000000, -0.9510565162951565288, 0.3090169943749382919 ) ) ;
#8808 = VECTOR ( 'NONE', #16185, 1000.000000000000000 ) ;
#8809 = VECTOR ( 'NONE', #11260, 1000.000000000000000 ) ;
#8810 = CARTESIAN_POINT ( 'NONE',  ( 1.139999999999995017, 6.898680348956876061E-16, 5.633200000000004870 ) ) ;
#8811 = DIRECTION ( 'NONE',  ( -1.000000000000000000, 0.000000000000000000, 0.000000000000000000 ) ) ;
#8812 = EDGE_CURVE ( 'NONE', #13330, #21564, #14071, .T. ) ;
#8813 = DIRECTION ( 'NONE',  ( -1.000000000000000000, -0.000000000000000000, -0.000000000000000000 ) ) ;
#8814 = ORIENTED_EDGE ( 'NONE', *, *, #9, .F. ) ;
#8815 = CYLINDRICAL_SURFACE ( 'NONE', #684, 88.00000000000000000 ) ;
#8816 = DIRECTION ( 'NONE',  ( 0.000000000000000000, 0.000000000000000000, -1.000000000000000000 ) ) ;
#8817 = DIRECTION ( 'NONE',  ( 0.000000000000000000, -0.2756373558169869509, -0.9612616959383223358 ) ) ;
#8818 = EDGE_CURVE ( 'NONE', #5168, #4256, #3680, .T. ) ;
#8819 = EDGE_LOOP ( 'NONE', ( #18453, #7870, #253, #3501 ) ) ;
#8820 = DIRECTION ( 'NONE',  ( 1.000000000000000000, 0.000000000000000000, 0.000000000000000000 ) ) ;
#8821 = ORIENTED_EDGE ( 'NONE', *, *, #13477, .F. ) ;
#8822 = AXIS2_PLACEMENT_3D ( 'NONE', #11859, #5126, #18607 ) ;
#8823 = DIRECTION ( 'NONE',  ( -1.000000000000000000, -0.000000000000000000, 0.000000000000000000 ) ) ;
#8824 = EDGE_CURVE ( 'NONE', #19781, #3530, #798, .T. ) ;
#8825 = ORIENTED_EDGE ( 'NONE', *, *, #423, .T. ) ;
#8826 = ORIENTED_EDGE ( 'NONE', *, *, #15537, .T. ) ;
#8827 = EDGE_CURVE ( 'NONE', #13950, #12094, #2140, .T. ) ;
#8828 = EDGE_CURVE ( 'NONE', #1297, #16358, #7119, .T. ) ;
#8829 = ORIENTED_EDGE ( 'NONE', *, *, #17755, .T. ) ;
#8830 = CARTESIAN_POINT ( 'NONE',  ( 0.000000000000000000, 71.33759994381961178, 58.88447872959011420 ) ) ;
#8831 = DIRECTION ( 'NONE',  ( 0.000000000000000000, 0.4067366430758011520, -0.9135454576426004225 ) ) ;
#8832 = CARTESIAN_POINT ( 'NONE',  ( 10.00000000000000000, -84.12297548659712731, 32.40974838672912028 ) ) ;
#8833 = FACE_OUTER_BOUND ( 'NONE', #19037, .T. ) ;
#8834 = CARTESIAN_POINT ( 'NONE',  ( 1.199999999999992628, 0.000000000000000000, 0.000000000000000000 ) ) ;
#8835 = EDGE_CURVE ( 'NONE', #1233, #1686, #11443, .T. ) ;
#8836 = CARTESIAN_POINT ( 'NONE',  ( 10.00000000000000000, 0.000000000000000000, 0.000000000000000000 ) ) ;
#8837 = DIRECTION ( 'NONE',  ( -1.000000000000000000, 0.000000000000000000, 0.000000000000000000 ) ) ;
#8838 = AXIS2_PLACEMENT_3D ( 'NONE', #12721, #21236, #6223 ) ;
#8839 = CARTESIAN_POINT ( 'NONE',  ( -7.440711023145909486, 0.000000000000000000, 0.000000000000000000 ) ) ;
#8840 = DIRECTION ( 'NONE',  ( -1.000000000000000000, 0.000000000000000000, 0.000000000000000000 ) ) ;
#8841 = ORIENTED_EDGE ( 'NONE', *, *, #5316, .T. ) ;
#8842 = CARTESIAN_POINT ( 'NONE',  ( 9.999999999999994671, 0.000000000000000000, 103.6249999999999716 ) ) ;
#8843 = VERTEX_POINT ( 'NONE', #8770 ) ;
#8844 = ORIENTED_EDGE ( 'NONE', *, *, #2861, .T. ) ;
#8845 = ORIENTED_EDGE ( 'NONE', *, *, #21212, .F. ) ;
#8846 = DIRECTION ( 'NONE',  ( 0.000000000000000000, 0.000000000000000000, 1.000000000000000000 ) ) ;
#8847 = ORIENTED_EDGE ( 'NONE', *, *, #9960, .T. ) ;
#8848 = AXIS2_PLACEMENT_3D ( 'NONE', #6726, #7040, #14987 ) ;
#8849 = ORIENTED_EDGE ( 'NONE', *, *, #15554, .T. ) ;
#8850 = DIRECTION ( 'NONE',  ( 1.000000000000000000, 0.000000000000000000, 0.000000000000000000 ) ) ;
#8851 = ORIENTED_EDGE ( 'NONE', *, *, #10419, .T. ) ;
#8852 = CARTESIAN_POINT ( 'NONE',  ( 0.000000000000000000, 0.000000000000000000, 0.000000000000000000 ) ) ;
#8853 = DIRECTION ( 'NONE',  ( 1.000000000000000000, -0.000000000000000000, 0.000000000000000000 ) ) ;
#8854 = DIRECTION ( 'NONE',  ( 0.000000000000000000, 0.4694715627858917495, -0.8829475928589264333 ) ) ;
#8855 = CARTESIAN_POINT ( 'NONE',  ( 0.000000000000000000, 81.32027326007924728, -44.08455690948973427 ) ) ;
#8856 = LINE ( 'NONE', #1799, #2336 ) ;
#8857 = CARTESIAN_POINT ( 'NONE',  ( 10.00000000000000000, -28.15804365424197897, 1.358152127005888055 ) ) ;
#8858 = DIRECTION ( 'NONE',  ( 0.000000000000000000, -1.000000000000000000, 0.000000000000000000 ) ) ;
#8859 = CARTESIAN_POINT ( 'NONE',  ( 1.129531546211711479, 6.886005254585696675E-16, 5.612499999999999822 ) ) ;
#8860 = ORIENTED_EDGE ( 'NONE', *, *, #8390, .T. ) ;
#8861 = CARTESIAN_POINT ( 'NONE',  ( 10.00000000000000000, -43.18649929580143976, -73.28107340219457910 ) ) ;
#8862 = DIRECTION ( 'NONE',  ( 1.000000000000000000, 0.000000000000000000, 0.000000000000000000 ) ) ;
#8863 = ORIENTED_EDGE ( 'NONE', *, *, #16482, .F. ) ;
#8864 = EDGE_CURVE ( 'NONE', #1297, #17743, #2624, .T. ) ;
#8865 = CARTESIAN_POINT ( 'NONE',  ( 0.000000000000000000, -47.19205848891816402, 74.27590198428104884 ) ) ;
#8866 = EDGE_LOOP ( 'NONE', ( #10993, #16457, #8944, #14114 ) ) ;
#8867 =( NAMED_UNIT ( * ) SI_UNIT ( $, .STERADIAN. ) SOLID_ANGLE_UNIT ( ) );
#8868 = CARTESIAN_POINT ( 'NONE',  ( -10.00000000000001243, 1.238117913937974462E-14, 101.1000000000000369 ) ) ;
#8869 = ORIENTED_EDGE ( 'NONE', *, *, #6750, .T. ) ;
#8870 = VERTEX_POINT ( 'NONE', #379 ) ;
#8871 = AXIS2_PLACEMENT_3D ( 'NONE', #14606, #14271, #13057 ) ;
#8872 = DIRECTION ( 'NONE',  ( 0.000000000000000000, 0.000000000000000000, 1.000000000000000000 ) ) ;
#8873 = CARTESIAN_POINT ( 'NONE',  ( 5.000000000000002665, 17.64925110578469258, 86.21197095186350623 ) ) ;
#8874 = ADVANCED_FACE ( 'NONE', ( #10636, #5462, #17386 ), #13848, .F. ) ;
#8875 = DIRECTION ( 'NONE',  ( 1.000000000000000000, 0.000000000000000000, 0.000000000000000000 ) ) ;
#8876 = DIRECTION ( 'NONE',  ( 1.000000000000000000, 0.000000000000000000, 0.000000000000000000 ) ) ;
#8877 = DIRECTION ( 'NONE',  ( 0.000000000000000000, -0.9945218953682744001, 0.1045284632676437564 ) ) ;
#8878 = CARTESIAN_POINT ( 'NONE',  ( -10.00000000000000000, 0.000000000000000000, 32.00000000000000000 ) ) ;
#8879 = CARTESIAN_POINT ( 'NONE',  ( 0.000000000000000000, 0.000000000000000000, 3.000000000000000000 ) ) ;
#8880 = DIRECTION ( 'NONE',  ( 1.000000000000000000, 0.000000000000000000, 0.000000000000000000 ) ) ;
#8881 = EDGE_LOOP ( 'NONE', ( #19689, #5167, #15685, #3796 ) ) ;
#8882 = FACE_OUTER_BOUND ( 'NONE', #5629, .T. ) ;
#8883 = ORIENTED_EDGE ( 'NONE', *, *, #3409, .T. ) ;
#8884 = DIRECTION ( 'NONE',  ( 0.000000000000000000, 0.000000000000000000, 1.000000000000000000 ) ) ;
#8885 = ORIENTED_EDGE ( 'NONE', *, *, #14559, .T. ) ;
#8886 = CARTESIAN_POINT ( 'NONE',  ( 10.00000000000000000, 69.25892805976580746, -49.38005998797770246 ) ) ;
#8887 = ADVANCED_FACE ( 'NONE', ( #20706 ), #14167, .F. ) ;
#8888 = CARTESIAN_POINT ( 'NONE',  ( 10.00000000000000000, -66.01871308925505843, 64.79170103522997692 ) ) ;
#8889 = ORIENTED_EDGE ( 'NONE', *, *, #9710, .T. ) ;
#8890 = ORIENTED_EDGE ( 'NONE', *, *, #11572, .T. ) ;
#8891 = VERTEX_POINT ( 'NONE', #15938 ) ;
#8892 = ORIENTED_EDGE ( 'NONE', *, *, #9628, .T. ) ;
#8893 = CARTESIAN_POINT ( 'NONE',  ( 5.000000000000002665, 35.18804927320529430, 80.65854690202691302 ) ) ;
#8894 = ORIENTED_EDGE ( 'NONE', *, *, #17166, .F. ) ;
#8895 = DIRECTION ( 'NONE',  ( 1.000000000000000000, -0.000000000000000000, 0.000000000000000000 ) ) ;
#8896 = CYLINDRICAL_SURFACE ( 'NONE', #10502, 92.50100000000000477 ) ;
#8897 = DIRECTION ( 'NONE',  ( 1.000000000000000000, 0.000000000000000000, 0.000000000000000000 ) ) ;
#8898 = DIRECTION ( 'NONE',  ( 0.000000000000000000, 0.5299192642331997938, 0.8480480961564290654 ) ) ;
#8899 = DIRECTION ( 'NONE',  ( -1.000000000000000000, -0.000000000000000000, -0.000000000000000000 ) ) ;
#8900 = EDGE_CURVE ( 'NONE', #4889, #239, #8281, .T. ) ;
#8901 = AXIS2_PLACEMENT_3D ( 'NONE', #2538, #6092, #15917 ) ;
#8902 = CARTESIAN_POINT ( 'NONE',  ( 10.00000000000000000, -69.25892805976475586, -49.38005998797915908 ) ) ;
#8903 = ORIENTED_EDGE ( 'NONE', *, *, #1638, .T. ) ;
#8904 = EDGE_CURVE ( 'NONE', #18616, #14552, #1570, .T. ) ;
#8905 = DIRECTION ( 'NONE',  ( -1.000000000000000000, -0.000000000000000000, -0.000000000000000000 ) ) ;
#8906 = AXIS2_PLACEMENT_3D ( 'NONE', #18575, #4870, #11497 ) ;
#8907 = DIRECTION ( 'NONE',  ( 0.000000000000000000, 0.000000000000000000, -1.000000000000000000 ) ) ;
#8908 = VECTOR ( 'NONE', #13342, 1000.000000000000000 ) ;
#8909 = DIRECTION ( 'NONE',  ( -1.000000000000000000, -0.000000000000000000, -0.000000000000000000 ) ) ;
#8910 = ORIENTED_EDGE ( 'NONE', *, *, #16516, .T. ) ;
#8911 = EDGE_CURVE ( 'NONE', #17874, #2596, #11811, .T. ) ;
#8912 = CARTESIAN_POINT ( 'NONE',  ( 0.000000000000000000, 0.000000000000000000, 0.000000000000000000 ) ) ;
#8913 = ADVANCED_FACE ( 'NONE', ( #16162 ), #1356, .F. ) ;
#8914 = EDGE_CURVE ( 'NONE', #10156, #16787, #6017, .T. ) ;
#8915 = EDGE_LOOP ( 'NONE', ( #13096, #18121, #14848, #12005 ) ) ;
#8916 = DIRECTION ( 'NONE',  ( 0.000000000000000000, 0.000000000000000000, 1.000000000000000000 ) ) ;
#8917 = EDGE_LOOP ( 'NONE', ( #15194, #11457, #4444, #16954 ) ) ;
#8918 = ADVANCED_FACE ( 'NONE', ( #2564 ), #21146, .T. ) ;
#8919 = EDGE_LOOP ( 'NONE', ( #10186, #5291, #20088, #9141 ) ) ;
#8920 = ORIENTED_EDGE ( 'NONE', *, *, #2281, .F. ) ;
#8921 = DIRECTION ( 'NONE',  ( 1.000000000000000000, 0.000000000000000000, 0.000000000000000000 ) ) ;
#8922 = ORIENTED_EDGE ( 'NONE', *, *, #6424, .F. ) ;
#8923 = CARTESIAN_POINT ( 'NONE',  ( 0.000000000000000000, 0.000000000000000000, 0.000000000000000000 ) ) ;
#8924 = AXIS2_PLACEMENT_3D ( 'NONE', #11668, #4933, #12577 ) ;
#8925 = VECTOR ( 'NONE', #18437, 1000.000000000000000 ) ;
#8926 = DIRECTION ( 'NONE',  ( -1.000000000000000000, 0.000000000000000000, 0.000000000000000000 ) ) ;
#8927 = DIRECTION ( 'NONE',  ( -1.000000000000000000, 0.000000000000000000, 0.000000000000000000 ) ) ;
#8928 = CARTESIAN_POINT ( 'NONE',  ( 10.00000000000000000, 3.728035544476225649, 84.97818067823770605 ) ) ;
#8929 = EDGE_CURVE ( 'NONE', #10036, #8447, #7776, .T. ) ;
#8930 = FACE_OUTER_BOUND ( 'NONE', #14037, .T. ) ;
#8931 = CARTESIAN_POINT ( 'NONE',  ( -10.00000000000000000, 0.000000000000000000, 0.000000000000000000 ) ) ;
#8932 = DIRECTION ( 'NONE',  ( 0.000000000000000000, -0.9945218953682721796, -0.1045284632676636571 ) ) ;
#8933 = CARTESIAN_POINT ( 'NONE',  ( -10.00000000000000000, 0.000000000000000000, 0.000000000000000000 ) ) ;
#8934 = EDGE_CURVE ( 'NONE', #9557, #12679, #1247, .T. ) ;
#8935 = LINE ( 'NONE', #5745, #13729 ) ;
#8936 = VECTOR ( 'NONE', #12683, 1000.000000000000000 ) ;
#8937 = ORIENTED_EDGE ( 'NONE', *, *, #12856, .F. ) ;
#8938 = EDGE_CURVE ( 'NONE', #7118, #9088, #17801, .T. ) ;
#8939 = DIRECTION ( 'NONE',  ( 1.000000000000000000, 0.000000000000000000, -0.000000000000000000 ) ) ;
#8940 = AXIS2_PLACEMENT_3D ( 'NONE', #4133, #10868, #11083 ) ;
#8941 = VERTEX_POINT ( 'NONE', #12733 ) ;
#8942 = VERTEX_POINT ( 'NONE', #9521 ) ;
#8943 = VECTOR ( 'NONE', #5489, 1000.000000000000000 ) ;
#8944 = ORIENTED_EDGE ( 'NONE', *, *, #18910, .F. ) ;
#8945 = CYLINDRICAL_SURFACE ( 'NONE', #19090, 88.00000000000000000 ) ;
#8946 = EDGE_CURVE ( 'NONE', #5948, #16620, #6349, .T. ) ;
#8947 = ORIENTED_EDGE ( 'NONE', *, *, #17683, .F. ) ;
#8948 = ORIENTED_EDGE ( 'NONE', *, *, #4517, .F. ) ;
#8949 = EDGE_CURVE ( 'NONE', #21757, #20880, #20625, .T. ) ;
#8950 = DIRECTION ( 'NONE',  ( 0.000000000000000000, -0.6427876096865456912, 0.7660444431189725734 ) ) ;
#8951 = VECTOR ( 'NONE', #12340, 1000.000000000000000 ) ;
#8952 = ORIENTED_EDGE ( 'NONE', *, *, #16081, .F. ) ;
#8953 = CARTESIAN_POINT ( 'NONE',  ( 10.00000000000000000, 22.77465461094674026, 15.41136296218094159 ) ) ;
#8954 = FACE_OUTER_BOUND ( 'NONE', #19097, .T. ) ;
#8955 = CIRCLE ( 'NONE', #19540, 32.00000000000000000 ) ;
#8956 = CARTESIAN_POINT ( 'NONE',  ( 10.00000000000000000, 31.75612719289740937, 3.943144139962659445 ) ) ;
#8957 = FACE_OUTER_BOUND ( 'NONE', #15741, .T. ) ;
#8958 = CARTESIAN_POINT ( 'NONE',  ( 0.000000000000000000, 0.000000000000000000, 0.000000000000000000 ) ) ;
#8959 = EDGE_CURVE ( 'NONE', #19484, #5341, #16493, .T. ) ;
#8960 = TOROIDAL_SURFACE ( 'NONE', #14244, 118.9000000000000199, 1.100000000000009859 ) ;
#8961 = CARTESIAN_POINT ( 'NONE',  ( 0.000000000000000000, -84.90234713953981327, -5.175025661884713912 ) ) ;
#8962 = DIRECTION ( 'NONE',  ( 0.000000000000000000, 0.9510565162951521989, 0.3090169943749513926 ) ) ;
#8963 = VERTEX_POINT ( 'NONE', #911 ) ;
#8964 = EDGE_CURVE ( 'NONE', #17498, #9215, #11403, .T. ) ;
#8965 = AXIS2_PLACEMENT_3D ( 'NONE', #7665, #3913, #14283 ) ;
#8966 = FACE_OUTER_BOUND ( 'NONE', #6445, .T. ) ;
#8967 = CIRCLE ( 'NONE', #7913, 45.00000000000000000 ) ;
#8968 = CARTESIAN_POINT ( 'NONE',  ( 10.00000000000000000, 84.33453774737672859, -11.08490790852044405 ) ) ;
#8969 = ORIENTED_EDGE ( 'NONE', *, *, #6250, .F. ) ;
#8970 = DIRECTION ( 'NONE',  ( 0.000000000000000000, 0.5299192642332061221, -0.8480480961564251796 ) ) ;
#8971 = ORIENTED_EDGE ( 'NONE', *, *, #20816, .F. ) ;
#8972 = LINE ( 'NONE', #17285, #2924 ) ;
#8973 = ORIENTED_EDGE ( 'NONE', *, *, #20850, .F. ) ;
#8974 = VERTEX_POINT ( 'NONE', #21354 ) ;
#8975 = DIRECTION ( 'NONE',  ( 0.000000000000000000, 0.000000000000000000, 1.000000000000000000 ) ) ;
#8976 = AXIS2_PLACEMENT_3D ( 'NONE', #7998, #14728, #13067 ) ;
#8977 = CARTESIAN_POINT ( 'NONE',  ( 10.00000000000000000, 0.000000000000000000, 0.000000000000000000 ) ) ;
#8978 = CARTESIAN_POINT ( 'NONE',  ( 0.000000000000000000, 91.49386717542239467, -13.61276130276895735 ) ) ;
#8979 = AXIS2_PLACEMENT_3D ( 'NONE', #1752, #90, #18874 ) ;
#8980 = CYLINDRICAL_SURFACE ( 'NONE', #220, 44.99999999999999289 ) ;
#8981 = DIRECTION ( 'NONE',  ( 0.000000000000000000, 0.000000000000000000, 1.000000000000000000 ) ) ;
#8982 = ADVANCED_FACE ( 'NONE', ( #16377 ), #6233, .F. ) ;
#8983 = AXIS2_PLACEMENT_3D ( 'NONE', #16880, #2651, #18219 ) ;
#8984 = DIRECTION ( 'NONE',  ( -1.000000000000000000, 0.000000000000000000, -0.000000000000000000 ) ) ;
#8985 = CARTESIAN_POINT ( 'NONE',  ( 8.899999999999989697, 0.000000000000000000, -101.1000000000000512 ) ) ;
#8986 = TOROIDAL_SURFACE ( 'NONE', #16033, 5.100000000000000533, 0.1000000000000000472 ) ;
#8987 = VERTEX_POINT ( 'NONE', #12949 ) ;
#8988 = CIRCLE ( 'NONE', #8296, 92.50100000000003320 ) ;
#8989 = DIRECTION ( 'NONE',  ( 1.000000000000000000, -0.000000000000000000, -0.000000000000000000 ) ) ;
#8990 = ORIENTED_EDGE ( 'NONE', *, *, #7188, .F. ) ;
#8991 = CARTESIAN_POINT ( 'NONE',  ( 10.00000000000000000, -75.45728100697571961, -39.26051685139143643 ) ) ;
#8992 = EDGE_LOOP ( 'NONE', ( #11317, #12388 ) ) ;
#8993 = DIRECTION ( 'NONE',  ( -1.000000000000000000, 0.000000000000000000, -0.000000000000000000 ) ) ;
#8994 = VECTOR ( 'NONE', #17327, 1000.000000000000000 ) ;
#8995 = CARTESIAN_POINT ( 'NONE',  ( 10.00000000000000000, -87.44637528609668209, 9.855528870798345054 ) ) ;
#8996 = VERTEX_POINT ( 'NONE', #19696 ) ;
#8997 = AXIS2_PLACEMENT_3D ( 'NONE', #14105, #407, #5604 ) ;
#8998 = FILL_AREA_STYLE_COLOUR ( '', #16274 ) ;
#8999 = AXIS2_PLACEMENT_3D ( 'NONE', #18050, #17942, #13064 ) ;
#9000 = ORIENTED_EDGE ( 'NONE', *, *, #21625, .F. ) ;
#9001 = VERTEX_POINT ( 'NONE', #4566 ) ;
#9002 = EDGE_LOOP ( 'NONE', ( #19362, #17573, #3953, #8643 ) ) ;
#9003 = DIRECTION ( 'NONE',  ( -1.000000000000000000, 0.000000000000000000, 0.000000000000000000 ) ) ;
#9004 = CARTESIAN_POINT ( 'NONE',  ( -10.00000000000000000, 0.000000000000000000, 0.000000000000000000 ) ) ;
#9005 = ORIENTED_EDGE ( 'NONE', *, *, #7411, .T. ) ;
#9006 = CARTESIAN_POINT ( 'NONE',  ( 10.00000000000000000, 0.000000000000000000, 0.000000000000000000 ) ) ;
#9007 = CARTESIAN_POINT ( 'NONE',  ( -10.00000000000001243, 103.6250000000000284, 0.000000000000000000 ) ) ;
#9008 = DIRECTION ( 'NONE',  ( 0.000000000000000000, 0.8290375725550428454, -0.5591929034707450175 ) ) ;
#9009 = AXIS2_PLACEMENT_3D ( 'NONE', #18184, #1162, #11759 ) ;
#9010 = LINE ( 'NONE', #6948, #18478 ) ;
#9011 = CYLINDRICAL_SURFACE ( 'NONE', #17604, 44.99999999999999289 ) ;
#9012 = EDGE_CURVE ( 'NONE', #5871, #3351, #153, .T. ) ;
#9013 = CIRCLE ( 'NONE', #7266, 9.999999999999998224 ) ;
#9014 = CIRCLE ( 'NONE', #9669, 11.99999999999999822 ) ;
#9015 = ORIENTED_EDGE ( 'NONE', *, *, #12692, .F. ) ;
#9016 = AXIS2_PLACEMENT_3D ( 'NONE', #11875, #5573, #12309 ) ;
#9017 = CYLINDRICAL_SURFACE ( 'NONE', #6350, 9.999999999999998224 ) ;
#9018 = CIRCLE ( 'NONE', #1616, 11.99999999999999822 ) ;
#9019 = DIRECTION ( 'NONE',  ( -1.000000000000000000, -0.000000000000000000, 0.000000000000000000 ) ) ;
#9020 = EDGE_CURVE ( 'NONE', #2027, #6083, #19559, .T. ) ;
#9021 = FACE_OUTER_BOUND ( 'NONE', #9352, .T. ) ;
#9022 = VERTEX_POINT ( 'NONE', #8101 ) ;
#9023 = CARTESIAN_POINT ( 'NONE',  ( -1.500000000000000000, -7.000000000000000000, 15.00000000000000000 ) ) ;
#9024 = ORIENTED_EDGE ( 'NONE', *, *, #20972, .T. ) ;
#9025 = FACE_OUTER_BOUND ( 'NONE', #17411, .T. ) ;
#9026 = ORIENTED_EDGE ( 'NONE', *, *, #2391, .T. ) ;
#9027 = EDGE_CURVE ( 'NONE', #12349, #17637, #6450, .T. ) ;
#9028 = ORIENTED_EDGE ( 'NONE', *, *, #16658, .T. ) ;
#9029 = AXIS2_PLACEMENT_3D ( 'NONE', #11718, #13377, #13475 ) ;
#9030 = ORIENTED_EDGE ( 'NONE', *, *, #1044, .F. ) ;
#9031 = FACE_OUTER_BOUND ( 'NONE', #10967, .T. ) ;
#9032 = CIRCLE ( 'NONE', #8681, 44.99999999999999289 ) ;
#9033 = ORIENTED_EDGE ( 'NONE', *, *, #18509, .F. ) ;
#9034 = AXIS2_PLACEMENT_3D ( 'NONE', #9797, #4843, #8487 ) ;
#9035 = CARTESIAN_POINT ( 'NONE',  ( -90.00000000000000000, 0.000000000000000000, 0.000000000000000000 ) ) ;
#9036 = LINE ( 'NONE', #2301, #5476 ) ;
#9037 = LINE ( 'NONE', #17122, #19149 ) ;
#9038 = DIRECTION ( 'NONE',  ( 1.000000000000000000, -0.000000000000000000, 0.000000000000000000 ) ) ;
#9039 = EDGE_CURVE ( 'NONE', #14663, #2607, #1458, .T. ) ;
#9040 = CYLINDRICAL_SURFACE ( 'NONE', #15991, 32.00000000000000000 ) ;
#9041 = EDGE_CURVE ( 'NONE', #9325, #5584, #13902, .T. ) ;
#9042 = DIRECTION ( 'NONE',  ( -1.000000000000000000, -0.000000000000000000, 0.000000000000000000 ) ) ;
#9043 = DIRECTION ( 'NONE',  ( 0.000000000000000000, 0.000000000000000000, 1.000000000000000000 ) ) ;
#9044 = EDGE_CURVE ( 'NONE', #14874, #19013, #14936, .T. ) ;
#9045 = DIRECTION ( 'NONE',  ( -1.000000000000000000, 0.000000000000000000, -0.000000000000000000 ) ) ;
#9046 = DIRECTION ( 'NONE',  ( 0.000000000000000000, 0.000000000000000000, 1.000000000000000000 ) ) ;
#9047 = EDGE_CURVE ( 'NONE', #5097, #18503, #12166, .T. ) ;
#9048 = CIRCLE ( 'NONE', #9384, 44.99999999999999289 ) ;
#9049 = ORIENTED_EDGE ( 'NONE', *, *, #20511, .F. ) ;
#9050 = DIRECTION ( 'NONE',  ( 1.000000000000000000, 0.000000000000000000, 0.000000000000000000 ) ) ;
#9051 = ORIENTED_EDGE ( 'NONE', *, *, #10970, .F. ) ;
#9052 = ORIENTED_EDGE ( 'NONE', *, *, #5250, .F. ) ;
#9053 = ORIENTED_EDGE ( 'NONE', *, *, #1373, .F. ) ;
#9054 = EDGE_CURVE ( 'NONE', #14985, #18973, #3120, .T. ) ;
#9055 = CARTESIAN_POINT ( 'NONE',  ( 10.00000000000000000, -76.53853822674008711, 43.42639941457088781 ) ) ;
#9056 = ORIENTED_EDGE ( 'NONE', *, *, #6475, .T. ) ;
#9057 = ORIENTED_EDGE ( 'NONE', *, *, #992, .T. ) ;
#9058 = ORIENTED_EDGE ( 'NONE', *, *, #595, .F. ) ;
#9059 = EDGE_CURVE ( 'NONE', #2259, #7118, #21677, .T. ) ;
#9060 = LINE ( 'NONE', #15365, #10858 ) ;
#9061 = VERTEX_POINT ( 'NONE', #15049 ) ;
#9062 = AXIS2_PLACEMENT_3D ( 'NONE', #17430, #3736, #1857 ) ;
#9063 = DIRECTION ( 'NONE',  ( 0.000000000000000000, 0.000000000000000000, 1.000000000000000000 ) ) ;
#9064 = CIRCLE ( 'NONE', #13665, 6.887500000000022382 ) ;
#9065 = FACE_OUTER_BOUND ( 'NONE', #15364, .T. ) ;
#9066 = LINE ( 'NONE', #5438, #13946 ) ;
#9067 = DIRECTION ( 'NONE',  ( 0.000000000000000000, 0.000000000000000000, 1.000000000000000000 ) ) ;
#9068 = CARTESIAN_POINT ( 'NONE',  ( 0.000000000000000000, 0.000000000000000000, 0.000000000000000000 ) ) ;
#9069 = CARTESIAN_POINT ( 'NONE',  ( -1.500000000000000000, -4.769696007084728073, 15.00000000000000000 ) ) ;
#9070 = CARTESIAN_POINT ( 'NONE',  ( 8.899999999999991473, 1.469576158976824618E-14, 120.0000000000000711 ) ) ;
#9071 = CARTESIAN_POINT ( 'NONE',  ( 10.00000000000000000, 29.47587714451039531, 82.91666097089130005 ) ) ;
#9072 = EDGE_CURVE ( 'NONE', #2087, #10036, #19581, .T. ) ;
#9073 = EDGE_LOOP ( 'NONE', ( #371, #5757, #20440, #20178 ) ) ;
#9074 = DIRECTION ( 'NONE',  ( -1.000000000000000000, -0.000000000000000000, -0.000000000000000000 ) ) ;
#9075 = AXIS2_PLACEMENT_3D ( 'NONE', #17569, #19111, #2422 ) ;
#9076 = AXIS2_PLACEMENT_3D ( 'NONE', #13176, #11649, #21375 ) ;
#9077 = VECTOR ( 'NONE', #5064, 1000.000000000000000 ) ;
#9078 = DIRECTION ( 'NONE',  ( 0.000000000000000000, 0.000000000000000000, 1.000000000000000000 ) ) ;
#9079 = VECTOR ( 'NONE', #9442, 1000.000000000000000 ) ;
#9080 = EDGE_CURVE ( 'NONE', #11720, #11543, #3223, .T. ) ;
#9081 = DIRECTION ( 'NONE',  ( 0.000000000000000000, 0.000000000000000000, 1.000000000000000000 ) ) ;
#9082 = ORIENTED_EDGE ( 'NONE', *, *, #1887, .T. ) ;
#9083 = DIRECTION ( 'NONE',  ( -1.000000000000000000, 0.000000000000000000, 0.000000000000000000 ) ) ;
#9084 = ADVANCED_FACE ( 'NONE', ( #5516 ), #540, .F. ) ;
#9085 = ORIENTED_EDGE ( 'NONE', *, *, #14904, .F. ) ;
#9086 =( LENGTH_UNIT ( ) NAMED_UNIT ( * ) SI_UNIT ( .MILLI., .METRE. ) );
#9087 = DIRECTION ( 'NONE',  ( 0.000000000000000000, 0.7431448254773909134, 0.6691306063588619013 ) ) ;
#9088 = VERTEX_POINT ( 'NONE', #7290 ) ;
#9089 = ORIENTED_EDGE ( 'NONE', *, *, #13237, .F. ) ;
#9090 = ADVANCED_FACE ( 'NONE', ( #9955 ), #4781, .F. ) ;
#9091 = DIRECTION ( 'NONE',  ( 0.000000000000000000, 0.000000000000000000, -1.000000000000000000 ) ) ;
#9092 = EDGE_CURVE ( 'NONE', #7542, #6615, #7584, .T. ) ;
#9093 = AXIS2_PLACEMENT_3D ( 'NONE', #16598, #20243, #5106 ) ;
#9094 = VECTOR ( 'NONE', #17291, 1000.000000000000000 ) ;
#9095 = CARTESIAN_POINT ( 'NONE',  ( 10.00000000000000000, 26.69209308833507777, 6.612652082459410607 ) ) ;
#9096 = LINE ( 'NONE', #4457, #7000 ) ;
#9097 = CIRCLE ( 'NONE', #12284, 44.99999999999999289 ) ;
#9098 = CARTESIAN_POINT ( 'NONE',  ( -7.395800000000001262, 0.000000000000000000, -105.0992000000000104 ) ) ;
#9099 = CIRCLE ( 'NONE', #17925, 44.99999999999999289 ) ;
#9100 = DIRECTION ( 'NONE',  ( 1.000000000000000000, 0.000000000000000000, 0.000000000000000000 ) ) ;
#9101 = CARTESIAN_POINT ( 'NONE',  ( 0.000000000000000000, 0.000000000000000000, -3.000000000000000000 ) ) ;
#9102 = LINE ( 'NONE', #6244, #13245 ) ;
#9103 = CARTESIAN_POINT ( 'NONE',  ( 10.00000000000000000, 89.12061559554334167, 24.77803214283572686 ) ) ;
#9104 = ORIENTED_EDGE ( 'NONE', *, *, #8406, .F. ) ;
#9105 = CARTESIAN_POINT ( 'NONE',  ( 5.000000000000000000, 52.25832601289194201, -70.80301803122729609 ) ) ;
#9106 = ORIENTED_EDGE ( 'NONE', *, *, #10253, .F. ) ;
#9107 = LINE ( 'NONE', #12637, #14019 ) ;
#9108 = VERTEX_POINT ( 'NONE', #18999 ) ;
#9109 = AXIS2_PLACEMENT_3D ( 'NONE', #2870, #7516, #9492 ) ;
#9110 = DIRECTION ( 'NONE',  ( -1.000000000000000000, -0.000000000000000000, -0.000000000000000000 ) ) ;
#9111 = CIRCLE ( 'NONE', #19014, 0.1000000000000002554 ) ;
#9112 = AXIS2_PLACEMENT_3D ( 'NONE', #5216, #16929, #5101 ) ;
#9113 = DIRECTION ( 'NONE',  ( 0.000000000000000000, 0.000000000000000000, 1.000000000000000000 ) ) ;
#9114 = CIRCLE ( 'NONE', #3478, 88.00000000000000000 ) ;
#9115 = VERTEX_POINT ( 'NONE', #20142 ) ;
#9116 = ORIENTED_EDGE ( 'NONE', *, *, #3262, .F. ) ;
#9117 = EDGE_LOOP ( 'NONE', ( #16750, #10065, #21778, #19902 ) ) ;
#9118 = ORIENTED_EDGE ( 'NONE', *, *, #2597, .F. ) ;
#9119 = CARTESIAN_POINT ( 'NONE',  ( -1.500000000000001332, 0.000000000000000000, 0.000000000000000000 ) ) ;
#9120 = DIRECTION ( 'NONE',  ( -1.000000000000000000, 0.000000000000000000, -0.000000000000000000 ) ) ;
#9121 = ORIENTED_EDGE ( 'NONE', *, *, #2878, .T. ) ;
#9122 = CARTESIAN_POINT ( 'NONE',  ( 0.000000000000000000, -7.240962358591786163, 31.16999300804312156 ) ) ;
#9123 = CARTESIAN_POINT ( 'NONE',  ( -1.399999999999998579, 9.184850993605175555E-16, 7.500000000000020428 ) ) ;
#9124 = DIRECTION ( 'NONE',  ( -1.000000000000000000, -0.000000000000000000, -0.000000000000000000 ) ) ;
#9125 = DIRECTION ( 'NONE',  ( 1.000000000000000000, 0.000000000000000000, 0.000000000000000000 ) ) ;
#9126 = DIRECTION ( 'NONE',  ( 0.000000000000000000, 0.000000000000000000, 1.000000000000000000 ) ) ;
#9127 = AXIS2_PLACEMENT_3D ( 'NONE', #15454, #3960, #2096 ) ;
#9128 = AXIS2_PLACEMENT_3D ( 'NONE', #964, #10907, #21188 ) ;
#9129 = ORIENTED_EDGE ( 'NONE', *, *, #10002, .T. ) ;
#9130 = AXIS2_PLACEMENT_3D ( 'NONE', #6979, #5319, #12045 ) ;
#9131 = DIRECTION ( 'NONE',  ( -1.000000000000000000, 0.000000000000000000, 0.000000000000000000 ) ) ;
#9132 = CARTESIAN_POINT ( 'NONE',  ( 0.000000000000000000, 0.000000000000000000, 0.000000000000000000 ) ) ;
#9133 = FACE_BOUND ( 'NONE', #1919, .T. ) ;
#9134 = EDGE_LOOP ( 'NONE', ( #20138, #13028, #1883, #7225 ) ) ;
#9135 = ORIENTED_EDGE ( 'NONE', *, *, #14796, .F. ) ;
#9136 = CARTESIAN_POINT ( 'NONE',  ( 1.500000000000001332, 0.000000000000000000, 0.000000000000000000 ) ) ;
#9137 = ORIENTED_EDGE ( 'NONE', *, *, #2382, .F. ) ;
#9138 = AXIS2_PLACEMENT_3D ( 'NONE', #1955, #21030, #18652 ) ;
#9139 = ORIENTED_EDGE ( 'NONE', *, *, #13124, .F. ) ;
#9140 = ADVANCED_FACE ( 'NONE', ( #8316 ), #2638, .T. ) ;
#9141 = ORIENTED_EDGE ( 'NONE', *, *, #15686, .T. ) ;
#9142 = AXIS2_PLACEMENT_3D ( 'NONE', #5590, #502, #13766 ) ;
#9143 = LINE ( 'NONE', #16105, #15377 ) ;
#9144 = CIRCLE ( 'NONE', #4567, 88.00000000000000000 ) ;
#9145 = ORIENTED_EDGE ( 'NONE', *, *, #16212, .F. ) ;
#9146 = CARTESIAN_POINT ( 'NONE',  ( 0.000000000000000000, 30.24235385705252099, -10.45944707835077381 ) ) ;
#9147 = CARTESIAN_POINT ( 'NONE',  ( -10.00000000000002309, 0.000000000000000000, 0.000000000000000000 ) ) ;
#9148 = DIRECTION ( 'NONE',  ( -1.000000000000000000, -0.000000000000000000, 0.000000000000000000 ) ) ;
#9149 = CARTESIAN_POINT ( 'NONE',  ( 10.00000000000000000, 27.26034713664097353, 4.817140289263753594 ) ) ;
#9150 = EDGE_CURVE ( 'NONE', #18200, #5699, #17819, .T. ) ;
#9151 = CARTESIAN_POINT ( 'NONE',  ( 10.00000000000000000, 56.34908017029559346, 63.71789861856471049 ) ) ;
#9152 = LINE ( 'NONE', #15899, #3432 ) ;
#9153 = DIRECTION ( 'NONE',  ( 1.000000000000000000, -0.000000000000000000, -0.000000000000000000 ) ) ;
#9154 = CARTESIAN_POINT ( 'NONE',  ( 0.000000000000000000, 84.12297548659704205, 12.59025161327141618 ) ) ;
#9155 = CARTESIAN_POINT ( 'NONE',  ( -10.00000000000000000, 0.000000000000000000, 0.000000000000000000 ) ) ;
#9156 = STYLED_ITEM ( 'NONE', ( #21163 ), #20897 ) ;
#9157 = CARTESIAN_POINT ( 'NONE',  ( 10.00000000000000000, 0.000000000000000000, 0.000000000000000000 ) ) ;
#9158 = ORIENTED_EDGE ( 'NONE', *, *, #19905, .T. ) ;
#9159 = ORIENTED_EDGE ( 'NONE', *, *, #21494, .T. ) ;
#9160 = VERTEX_POINT ( 'NONE', #338 ) ;
#9161 = ORIENTED_EDGE ( 'NONE', *, *, #2940, .T. ) ;
#9162 = EDGE_CURVE ( 'NONE', #15688, #12744, #7946, .T. ) ;
#9163 = EDGE_CURVE ( 'NONE', #15191, #4590, #193, .T. ) ;
#9164 = VERTEX_POINT ( 'NONE', #10594 ) ;
#9165 = FACE_OUTER_BOUND ( 'NONE', #13656, .T. ) ;
#9166 = ORIENTED_EDGE ( 'NONE', *, *, #3982, .T. ) ;
#9167 = VECTOR ( 'NONE', #17167, 1000.000000000000000 ) ;
#9168 = CARTESIAN_POINT ( 'NONE',  ( 10.00000000000000000, 0.000000000000000000, 0.000000000000000000 ) ) ;
#9169 = CARTESIAN_POINT ( 'NONE',  ( 10.00000000000000000, 0.000000000000000000, 0.000000000000000000 ) ) ;
#9170 = DIRECTION ( 'NONE',  ( 0.000000000000000000, 0.000000000000000000, -1.000000000000000000 ) ) ;
#9171 = CARTESIAN_POINT ( 'NONE',  ( -10.00000000000000000, 0.000000000000000000, 0.000000000000000000 ) ) ;
#9172 = DIRECTION ( 'NONE',  ( 1.000000000000000000, -0.000000000000000000, -0.000000000000000000 ) ) ;
#9173 = CARTESIAN_POINT ( 'NONE',  ( 10.00000000000000000, 0.000000000000000000, 0.000000000000000000 ) ) ;
#9174 = DIRECTION ( 'NONE',  ( 0.000000000000000000, 0.000000000000000000, 1.000000000000000000 ) ) ;
#9175 = EDGE_CURVE ( 'NONE', #16026, #5950, #14647, .T. ) ;
#9176 = CARTESIAN_POINT ( 'NONE',  ( 10.00000000000000000, -78.83848282823873888, -48.38314403117582430 ) ) ;
#9177 = VERTEX_POINT ( 'NONE', #15565 ) ;
#9178 = EDGE_CURVE ( 'NONE', #8545, #17704, #12246, .T. ) ;
#9179 = FACE_OUTER_BOUND ( 'NONE', #14977, .T. ) ;
#9180 = AXIS2_PLACEMENT_3D ( 'NONE', #8045, #19641, #7925 ) ;
#9181 = LINE ( 'NONE', #9393, #21813 ) ;
#9182 = DIRECTION ( 'NONE',  ( -1.000000000000000000, -0.000000000000000000, -0.000000000000000000 ) ) ;
#9183 = EDGE_CURVE ( 'NONE', #16361, #7513, #17449, .T. ) ;
#9184 = ORIENTED_EDGE ( 'NONE', *, *, #9072, .F. ) ;
#9185 = ADVANCED_FACE ( 'NONE', ( #11141 ), #860, .F. ) ;
#9186 = CARTESIAN_POINT ( 'NONE',  ( 10.00000000000000000, 79.66702613806774025, -29.80527447819464371 ) ) ;
#9187 = VERTEX_POINT ( 'NONE', #7720 ) ;
#9188 = CARTESIAN_POINT ( 'NONE',  ( 10.00000000000000000, 60.65655256511237781, 59.63197188857542841 ) ) ;
#9189 = EDGE_CURVE ( 'NONE', #5362, #11867, #1243, .T. ) ;
#9190 = CIRCLE ( 'NONE', #3563, 44.99999999999999289 ) ;
#9191 = ORIENTED_EDGE ( 'NONE', *, *, #5166, .T. ) ;
#9192 = ORIENTED_EDGE ( 'NONE', *, *, #6648, .T. ) ;
#9193 = DIRECTION ( 'NONE',  ( -1.000000000000000000, 0.000000000000000000, -0.000000000000000000 ) ) ;
#9194 = DIRECTION ( 'NONE',  ( 1.000000000000000000, 0.000000000000000000, 0.000000000000000000 ) ) ;
#9195 = DIRECTION ( 'NONE',  ( -1.000000000000000000, 0.000000000000000000, -0.000000000000000000 ) ) ;
#9196 = DIRECTION ( 'NONE',  ( -1.000000000000000000, -0.000000000000000000, 0.000000000000000000 ) ) ;
#9197 = CARTESIAN_POINT ( 'NONE',  ( 0.000000000000000000, -30.61448696004446290, -9.314139153634542367 ) ) ;
#9198 = MECHANICAL_DESIGN_GEOMETRIC_PRESENTATION_REPRESENTATION (  '', ( #11697 ), #13085 ) ;
#9199 = LINE ( 'NONE', #5791, #19550 ) ;
#9200 = DIRECTION ( 'NONE',  ( -1.000000000000000000, 0.000000000000000000, 0.000000000000000000 ) ) ;
#9201 = CARTESIAN_POINT ( 'NONE',  ( 10.00000000000000000, -91.70173545986527586, 12.13370160540012499 ) ) ;
#9202 = EDGE_CURVE ( 'NONE', #6772, #11604, #20761, .T. ) ;
#9203 = DIRECTION ( 'NONE',  ( 0.000000000000000000, 0.000000000000000000, 1.000000000000000000 ) ) ;
#9204 = ORIENTED_EDGE ( 'NONE', *, *, #12799, .T. ) ;
#9205 = EDGE_CURVE ( 'NONE', #11959, #16727, #6067, .T. ) ;
#9206 = DIRECTION ( 'NONE',  ( 0.000000000000000000, 0.000000000000000000, 1.000000000000000000 ) ) ;
#9207 = ORIENTED_EDGE ( 'NONE', *, *, #3313, .T. ) ;
#9208 = ADVANCED_FACE ( 'NONE', ( #12681 ), #20864, .F. ) ;
#9209 = DIRECTION ( 'NONE',  ( -0.000000000000000000, -0.000000000000000000, -1.000000000000000000 ) ) ;
#9210 = ORIENTED_EDGE ( 'NONE', *, *, #15270, .T. ) ;
#9211 = CARTESIAN_POINT ( 'NONE',  ( 10.00000000000000000, -17.70753755129023332, -21.03896658273990639 ) ) ;
#9212 = VECTOR ( 'NONE', #17071, 1000.000000000000000 ) ;
#9213 = DIRECTION ( 'NONE',  ( 0.000000000000000000, 0.000000000000000000, 1.000000000000000000 ) ) ;
#9214 = ORIENTED_EDGE ( 'NONE', *, *, #20032, .F. ) ;
#9215 = VERTEX_POINT ( 'NONE', #12573 ) ;
#9216 = ADVANCED_FACE ( 'NONE', ( #14345 ), #1583, .T. ) ;
#9217 = ORIENTED_EDGE ( 'NONE', *, *, #9281, .T. ) ;
#9218 = ORIENTED_EDGE ( 'NONE', *, *, #9437, .T. ) ;
#9219 = DIRECTION ( 'NONE',  ( 0.000000000000000000, 0.5877852522924689183, 0.8090169943749505599 ) ) ;
#9220 = DIRECTION ( 'NONE',  ( -1.000000000000000000, -0.000000000000000000, 0.000000000000000000 ) ) ;
#9221 = ORIENTED_EDGE ( 'NONE', *, *, #21343, .F. ) ;
#9222 = FACE_OUTER_BOUND ( 'NONE', #11517, .T. ) ;
#9223 = CYLINDRICAL_SURFACE ( 'NONE', #3461, 44.99999999999998579 ) ;
#9224 = CARTESIAN_POINT ( 'NONE',  ( 0.000000000000000000, 0.000000000000000000, 9.999999999999998224 ) ) ;
#9225 = DIRECTION ( 'NONE',  ( 0.000000000000000000, 0.000000000000000000, -1.000000000000000000 ) ) ;
#9226 = CARTESIAN_POINT ( 'NONE',  ( 5.000000000000000000, 27.40684453873989668, -16.51862198941980608 ) ) ;
#9227 = EDGE_LOOP ( 'NONE', ( #20929, #10006, #3600, #22 ) ) ;
#9228 = CYLINDRICAL_SURFACE ( 'NONE', #11282, 5.000000000000000000 ) ;
#9229 = DIRECTION ( 'NONE',  ( -1.000000000000000000, -0.000000000000000000, -0.000000000000000000 ) ) ;
#9230 = EDGE_CURVE ( 'NONE', #20799, #19543, #9036, .T. ) ;
#9231 = FACE_OUTER_BOUND ( 'NONE', #3043, .T. ) ;
#9232 = EDGE_LOOP ( 'NONE', ( #11707, #21639, #4024, #2353 ) ) ;
#9233 = VECTOR ( 'NONE', #14692, 1000.000000000000000 ) ;
#9234 = DIRECTION ( 'NONE',  ( 0.000000000000000000, 0.000000000000000000, -1.000000000000000000 ) ) ;
#9235 = ORIENTED_EDGE ( 'NONE', *, *, #17055, .F. ) ;
#9236 = DIRECTION ( 'NONE',  ( 0.000000000000000000, 0.000000000000000000, 1.000000000000000000 ) ) ;
#9237 = ORIENTED_EDGE ( 'NONE', *, *, #4169, .T. ) ;
#9238 = ORIENTED_EDGE ( 'NONE', *, *, #14210, .T. ) ;
#9239 = ORIENTED_EDGE ( 'NONE', *, *, #6546, .T. ) ;
#9240 = DIRECTION ( 'NONE',  ( 1.000000000000000000, 0.000000000000000000, 0.000000000000000000 ) ) ;
#9241 = ORIENTED_EDGE ( 'NONE', *, *, #7580, .T. ) ;
#9242 = DIRECTION ( 'NONE',  ( 1.000000000000000000, 0.000000000000000000, 0.000000000000000000 ) ) ;
#9243 = DIRECTION ( 'NONE',  ( 1.000000000000000000, 0.000000000000000000, 0.000000000000000000 ) ) ;
#9244 = DIRECTION ( 'NONE',  ( 0.000000000000000000, 0.8660254037844398178, -0.4999999999999980016 ) ) ;
#9245 = DIRECTION ( 'NONE',  ( 1.000000000000000000, 0.000000000000000000, 0.000000000000000000 ) ) ;
#9246 = CIRCLE ( 'NONE', #2212, 45.00000000000000000 ) ;
#9247 = DIRECTION ( 'NONE',  ( 0.000000000000000000, 0.000000000000000000, 1.000000000000000000 ) ) ;
#9248 = CARTESIAN_POINT ( 'NONE',  ( 10.00000000000000000, 78.04699792498210797, -49.64978465107211747 ) ) ;
#9249 = DIRECTION ( 'NONE',  ( 1.000000000000000000, 0.000000000000000000, 0.000000000000000000 ) ) ;
#9250 = AXIS2_PLACEMENT_3D ( 'NONE', #21418, #13022, #19766 ) ;
#9251 = DIRECTION ( 'NONE',  ( 1.000000000000000000, -0.000000000000000000, -0.000000000000000000 ) ) ;
#9252 = DIRECTION ( 'NONE',  ( 1.000000000000000000, 0.000000000000000000, 0.000000000000000000 ) ) ;
#9253 = CARTESIAN_POINT ( 'NONE',  ( 10.00000000000000000, -56.34908017029602689, 63.71789861856433390 ) ) ;
#9254 = ORIENTED_EDGE ( 'NONE', *, *, #12026, .F. ) ;
#9255 = CIRCLE ( 'NONE', #8216, 44.99999999999998579 ) ;
#9256 = VERTEX_POINT ( 'NONE', #19103 ) ;
#9257 = PRODUCT_DEFINITION ( 'UNKNOWN', '', #20527, #17126 ) ;
#9258 = ORIENTED_EDGE ( 'NONE', *, *, #8628, .T. ) ;
#9259 = AXIS2_PLACEMENT_3D ( 'NONE', #2195, #12250, #10372 ) ;
#9260 = VECTOR ( 'NONE', #4956, 1000.000000000000000 ) ;
#9261 = ORIENTED_EDGE ( 'NONE', *, *, #16892, .F. ) ;
#9262 = AXIS2_PLACEMENT_3D ( 'NONE', #7442, #264, #2239 ) ;
#9263 = EDGE_LOOP ( 'NONE', ( #20704, #6191, #6983, #3558 ) ) ;
#9264 = LINE ( 'NONE', #4422, #12282 ) ;
#9265 = ORIENTED_EDGE ( 'NONE', *, *, #4058, .T. ) ;
#9266 = CARTESIAN_POINT ( 'NONE',  ( 10.00000000000000000, -33.95793648385871677, 86.04239391577979745 ) ) ;
#9267 = CARTESIAN_POINT ( 'NONE',  ( 0.000000000000000000, -72.53479564998815476, 44.42851404693331574 ) ) ;
#9268 = CARTESIAN_POINT ( 'NONE',  ( 10.00000000000000000, -41.21966518006011881, 82.80926399530274296 ) ) ;
#9269 = AXIS2_PLACEMENT_3D ( 'NONE', #19208, #10806, #9363 ) ;
#9270 = DIRECTION ( 'NONE',  ( 0.000000000000000000, 0.06975647374412546897, -0.9975640502598241977 ) ) ;
#9271 = DIRECTION ( 'NONE',  ( 0.000000000000000000, -0.1391731009600725433, 0.9902680687415692518 ) ) ;
#9272 = CYLINDRICAL_SURFACE ( 'NONE', #1996, 45.00000000000000000 ) ;
#9273 = FACE_OUTER_BOUND ( 'NONE', #1156, .T. ) ;
#9274 = CARTESIAN_POINT ( 'NONE',  ( 10.00000000000000000, 81.32027326007866463, 44.08455690949082850 ) ) ;
#9275 = CARTESIAN_POINT ( 'NONE',  ( 10.00000000000000000, -68.36541360927154187, -50.60987712331774446 ) ) ;
#9276 = AXIS2_PLACEMENT_3D ( 'NONE', #18414, #3259, #20065 ) ;
#9277 = EDGE_CURVE ( 'NONE', #16302, #20772, #17557, .T. ) ;
#9278 = ORIENTED_EDGE ( 'NONE', *, *, #14531, .F. ) ;
#9279 = CIRCLE ( 'NONE', #16708, 88.00000000000000000 ) ;
#9280 = DIRECTION ( 'NONE',  ( 1.000000000000000000, 0.000000000000000000, 0.000000000000000000 ) ) ;
#9281 = EDGE_CURVE ( 'NONE', #14246, #12590, #8988, .T. ) ;
#9282 = DIRECTION ( 'NONE',  ( 0.000000000000000000, 0.000000000000000000, 1.000000000000000000 ) ) ;
#9283 = FACE_OUTER_BOUND ( 'NONE', #2241, .T. ) ;
#9284 = CIRCLE ( 'NONE', #18842, 12.00000000000000000 ) ;
#9285 = VERTEX_POINT ( 'NONE', #2412 ) ;
#9286 = DIRECTION ( 'NONE',  ( -1.000000000000000000, -0.000000000000000000, 0.000000000000000000 ) ) ;
#9287 = ORIENTED_EDGE ( 'NONE', *, *, #18292, .F. ) ;
#9288 = ORIENTED_EDGE ( 'NONE', *, *, #12198, .T. ) ;
#9289 = APPLICATION_PROTOCOL_DEFINITION ( 'draft international standard', 'automotive_design', 1998, #5318 ) ;
#9290 = EDGE_CURVE ( 'NONE', #1656, #5948, #11115, .T. ) ;
#9291 = AXIS2_PLACEMENT_3D ( 'NONE', #3456, #18486, #3667 ) ;
#9292 = CYLINDRICAL_SURFACE ( 'NONE', #11411, 92.50100000000000477 ) ;
#9293 = ORIENTED_EDGE ( 'NONE', *, *, #11060, .F. ) ;
#9294 = EDGE_LOOP ( 'NONE', ( #10198, #2821, #6524, #21562 ) ) ;
#9295 = CARTESIAN_POINT ( 'NONE',  ( -126.5000000000000000, 1.549178200921401833E-14, -3.000000000000000000 ) ) ;
#9296 = AXIS2_PLACEMENT_3D ( 'NONE', #21269, #16290, #18300 ) ;
#9297 = CYLINDRICAL_SURFACE ( 'NONE', #8465, 27.49900000000000233 ) ;
#9298 = CARTESIAN_POINT ( 'NONE',  ( 5.000000000000000000, 85.22372865846293166, 21.92979875759657560 ) ) ;
#9299 = DIRECTION ( 'NONE',  ( -1.000000000000000000, -0.000000000000000000, -0.000000000000000000 ) ) ;
#9300 = DIRECTION ( 'NONE',  ( 1.000000000000000000, 0.000000000000000000, 0.000000000000000000 ) ) ;
#9301 = LINE ( 'NONE', #2474, #13924 ) ;
#9302 = CYLINDRICAL_SURFACE ( 'NONE', #17405, 45.00000000000000000 ) ;
#9303 = FACE_OUTER_BOUND ( 'NONE', #11369, .T. ) ;
#9304 = DIRECTION ( 'NONE',  ( -1.000000000000000000, -0.000000000000000000, -0.000000000000000000 ) ) ;
#9305 = AXIS2_PLACEMENT_3D ( 'NONE', #19479, #17394, #19379 ) ;
#9306 = EDGE_CURVE ( 'NONE', #17849, #14874, #19927, .T. ) ;
#9307 = EDGE_CURVE ( 'NONE', #16742, #20271, #2744, .T. ) ;
#9308 = EDGE_CURVE ( 'NONE', #9851, #12482, #6543, .T. ) ;
#9309 = VERTEX_POINT ( 'NONE', #9358 ) ;
#9310 = DIRECTION ( 'NONE',  ( 0.000000000000000000, 0.000000000000000000, 1.000000000000000000 ) ) ;
#9311 = VECTOR ( 'NONE', #6044, 1000.000000000000227 ) ;
#9312 = EDGE_CURVE ( 'NONE', #13478, #14138, #10917, .T. ) ;
#9313 = ORIENTED_EDGE ( 'NONE', *, *, #12404, .F. ) ;
#9314 = CIRCLE ( 'NONE', #2275, 88.00000000000000000 ) ;
#9315 = DIRECTION ( 'NONE',  ( 0.8831157194574072999, 5.745494457773168027E-17, 0.4691552259617553511 ) ) ;
#9316 =( LENGTH_UNIT ( ) NAMED_UNIT ( * ) SI_UNIT ( .MILLI., .METRE. ) );
#9317 = FACE_OUTER_BOUND ( 'NONE', #9263, .T. ) ;
#9318 = VERTEX_POINT ( 'NONE', #16225 ) ;
#9319 =( NAMED_UNIT ( * ) SI_UNIT ( $, .STERADIAN. ) SOLID_ANGLE_UNIT ( ) );
#9320 = EDGE_CURVE ( 'NONE', #16026, #13465, #15992, .T. ) ;
#9321 = AXIS2_PLACEMENT_3D ( 'NONE', #4343, #12739, #2358 ) ;
#9322 = ORIENTED_EDGE ( 'NONE', *, *, #20647, .F. ) ;
#9323 = VERTEX_POINT ( 'NONE', #2627 ) ;
#9324 = CIRCLE ( 'NONE', #16748, 88.00000000000000000 ) ;
#9325 = VERTEX_POINT ( 'NONE', #16110 ) ;
#9326 = DIRECTION ( 'NONE',  ( 0.000000000000000000, 0.5877852522924740253, -0.8090169943749466741 ) ) ;
#9327 = CARTESIAN_POINT ( 'NONE',  ( -1.500000000000001332, 9.123618653647806797E-16, 7.400000000000019895 ) ) ;
#9328 = ORIENTED_EDGE ( 'NONE', *, *, #14624, .T. ) ;
#9329 = ADVANCED_FACE ( 'NONE', ( #974 ), #9912, .T. ) ;
#9330 = VECTOR ( 'NONE', #17718, 1000.000000000000000 ) ;
#9331 = DIRECTION ( 'NONE',  ( 1.000000000000000000, 0.000000000000000000, 0.000000000000000000 ) ) ;
#9332 = CARTESIAN_POINT ( 'NONE',  ( 0.000000000000000000, 0.000000000000000000, 25.00000000000000000 ) ) ;
#9333 = DIRECTION ( 'NONE',  ( 0.000000000000000000, 1.000000000000000000, -1.224646799147353207E-16 ) ) ;
#9334 = CARTESIAN_POINT ( 'NONE',  ( 0.000000000000000000, -87.17509410653646285, 30.93441398372555540 ) ) ;
#9335 = AXIS2_PLACEMENT_3D ( 'NONE', #12036, #17121, #15458 ) ;
#9336 = DIRECTION ( 'NONE',  ( 1.000000000000000000, -0.000000000000000000, 0.000000000000000000 ) ) ;
#9337 = EDGE_LOOP ( 'NONE', ( #608, #19925, #12243, #2705 ) ) ;
#9338 = CARTESIAN_POINT ( 'NONE',  ( 10.00000000000000000, 9.646732466565339337, 84.51112348751853176 ) ) ;
#9339 = EDGE_CURVE ( 'NONE', #2427, #4091, #6897, .T. ) ;
#9340 = FACE_OUTER_BOUND ( 'NONE', #21272, .T. ) ;
#9341 = AXIS2_PLACEMENT_3D ( 'NONE', #4165, #10902, #17653 ) ;
#9342 = CARTESIAN_POINT ( 'NONE',  ( 10.00000000000000000, -69.25892805976543798, 49.38005998797819274 ) ) ;
#9343 = AXIS2_PLACEMENT_3D ( 'NONE', #5110, #20144, #246 ) ;
#9344 = ORIENTED_EDGE ( 'NONE', *, *, #6556, .T. ) ;
#9345 = CARTESIAN_POINT ( 'NONE',  ( -6.500000000000014211, 60.00000000000001421, 0.000000000000000000 ) ) ;
#9346 = ORIENTED_EDGE ( 'NONE', *, *, #12564, .T. ) ;
#9347 = DIRECTION ( 'NONE',  ( -1.000000000000000000, 0.000000000000000000, 0.000000000000000000 ) ) ;
#9348 = CIRCLE ( 'NONE', #16059, 27.49900000000000588 ) ;
#9349 = VERTEX_POINT ( 'NONE', #19761 ) ;
#9350 = EDGE_CURVE ( 'NONE', #20994, #3210, #10395, .T. ) ;
#9351 = ORIENTED_EDGE ( 'NONE', *, *, #8792, .F. ) ;
#9352 = EDGE_LOOP ( 'NONE', ( #18042, #8343, #17061, #13898 ) ) ;
#9353 = CIRCLE ( 'NONE', #3964, 92.50100000000003320 ) ;
#9354 = LINE ( 'NONE', #15665, #10751 ) ;
#9355 = EDGE_CURVE ( 'NONE', #19336, #993, #19236, .T. ) ;
#9356 = ORIENTED_EDGE ( 'NONE', *, *, #10171, .F. ) ;
#9357 = DIRECTION ( 'NONE',  ( 1.000000000000000000, 0.000000000000000000, 0.000000000000000000 ) ) ;
#9358 = CARTESIAN_POINT ( 'NONE',  ( 0.000000000000000000, 87.44637528609675314, -9.855528870797693131 ) ) ;
#9359 = DIRECTION ( 'NONE',  ( -0.000000000000000000, 1.000000000000000000, -0.000000000000000000 ) ) ;
#9360 = AXIS2_PLACEMENT_3D ( 'NONE', #11884, #1829, #15299 ) ;
#9361 = EDGE_CURVE ( 'NONE', #17526, #1297, #9692, .T. ) ;
#9362 = AXIS2_PLACEMENT_3D ( 'NONE', #15722, #5778, #7536 ) ;
#9363 = DIRECTION ( 'NONE',  ( 0.000000000000000000, -0.7431448254773997952, 0.6691306063588520203 ) ) ;
#9364 = AXIS2_PLACEMENT_3D ( 'NONE', #10317, #7123, #17393 ) ;
#9365 = EDGE_CURVE ( 'NONE', #21408, #4382, #1515, .T. ) ;
#9366 = DIRECTION ( 'NONE',  ( 0.000000000000000000, 0.000000000000000000, -1.000000000000000000 ) ) ;
#9367 = DIRECTION ( 'NONE',  ( -1.000000000000000000, 0.000000000000000000, -0.000000000000000000 ) ) ;
#9368 = DIRECTION ( 'NONE',  ( 0.000000000000000000, 0.000000000000000000, -1.000000000000000000 ) ) ;
#9369 = DIRECTION ( 'NONE',  ( 0.000000000000000000, 0.8290375725550390706, 0.5591929034707506796 ) ) ;
#9370 = DIRECTION ( 'NONE',  ( 0.000000000000000000, 0.9510565162951523099, 0.3090169943749513926 ) ) ;
#9371 = VERTEX_POINT ( 'NONE', #14557 ) ;
#9372 = ORIENTED_EDGE ( 'NONE', *, *, #5184, .T. ) ;
#9373 = EDGE_LOOP ( 'NONE', ( #20303, #17545, #8427, #16921 ) ) ;
#9374 = VECTOR ( 'NONE', #19645, 1000.000000000000000 ) ;
#9375 = ORIENTED_EDGE ( 'NONE', *, *, #15955, .T. ) ;
#9376 = ORIENTED_EDGE ( 'NONE', *, *, #4003, .F. ) ;
#9377 = DIRECTION ( 'NONE',  ( -1.000000000000000000, -0.000000000000000000, -0.000000000000000000 ) ) ;
#9378 = EDGE_LOOP ( 'NONE', ( #9660, #12898, #323, #6232 ) ) ;
#9379 = DIRECTION ( 'NONE',  ( 1.000000000000000000, 0.000000000000000000, 0.000000000000000000 ) ) ;
#9380 = CARTESIAN_POINT ( 'NONE',  ( 0.000000000000000000, 0.000000000000000000, 0.000000000000000000 ) ) ;
#9381 = DIRECTION ( 'NONE',  ( 1.000000000000000000, 0.000000000000000000, 0.000000000000000000 ) ) ;
#9382 = CARTESIAN_POINT ( 'NONE',  ( 0.000000000000000000, 0.000000000000000000, 0.000000000000000000 ) ) ;
#9383 = LINE ( 'NONE', #19451, #18651 ) ;
#9384 = AXIS2_PLACEMENT_3D ( 'NONE', #9923, #8909, #17329 ) ;
#9385 = CARTESIAN_POINT ( 'NONE',  ( 0.000000000000000000, 80.18694381077108346, 28.37681241246682973 ) ) ;
#9386 = PRESENTATION_LAYER_ASSIGNMENT (  '', '', ( #15762 ) ) ;
#9387 = DIRECTION ( 'NONE',  ( 0.000000000000000000, 0.000000000000000000, -1.000000000000000000 ) ) ;
#9388 = CARTESIAN_POINT ( 'NONE',  ( 10.00000000000000000, 0.000000000000000000, 0.000000000000000000 ) ) ;
#9389 = CARTESIAN_POINT ( 'NONE',  ( -10.00000000000000000, 0.000000000000000000, 0.000000000000000000 ) ) ;
#9390 = EDGE_LOOP ( 'NONE', ( #20324, #1132, #21296, #17698 ) ) ;
#9391 = CARTESIAN_POINT ( 'NONE',  ( 5.000000000000000000, 69.74988376404020585, 53.65588238863360715 ) ) ;
#9392 = ORIENTED_EDGE ( 'NONE', *, *, #12177, .F. ) ;
#9393 = CARTESIAN_POINT ( 'NONE',  ( 10.00000000000000000, 91.70173545986537533, -12.13370160539944287 ) ) ;
#9394 = CARTESIAN_POINT ( 'NONE',  ( 0.000000000000000000, 0.000000000000000000, 0.000000000000000000 ) ) ;
#9395 = VERTEX_POINT ( 'NONE', #8263 ) ;
#9396 = DIRECTION ( 'NONE',  ( 0.000000000000000000, 0.000000000000000000, 1.000000000000000000 ) ) ;
#9397 = VERTEX_POINT ( 'NONE', #19859 ) ;
#9398 = ORIENTED_EDGE ( 'NONE', *, *, #3131, .F. ) ;
#9399 = AXIS2_PLACEMENT_3D ( 'NONE', #8408, #20552, #5415 ) ;
#9400 = APPLICATION_PROTOCOL_DEFINITION ( 'draft international standard', 'automotive_design', 1998, #16715 ) ;
#9401 = DIRECTION ( 'NONE',  ( -1.000000000000000000, 0.000000000000000000, 0.000000000000000000 ) ) ;
#9402 = ORIENTED_EDGE ( 'NONE', *, *, #7888, .T. ) ;
#9403 = EDGE_CURVE ( 'NONE', #20730, #3351, #18215, .T. ) ;
#9404 = ORIENTED_EDGE ( 'NONE', *, *, #16868, .F. ) ;
#9405 = DIRECTION ( 'NONE',  ( 0.000000000000000000, 0.000000000000000000, -1.000000000000000000 ) ) ;
#9406 = DIRECTION ( 'NONE',  ( -1.000000000000000000, 0.000000000000000000, 0.000000000000000000 ) ) ;
#9407 = DIRECTION ( 'NONE',  ( 0.000000000000000000, 0.9510565162951523099, 0.3090169943749512260 ) ) ;
#9408 = DIRECTION ( 'NONE',  ( 0.000000000000000000, 0.6946583704589935904, 0.7193398003386546335 ) ) ;
#9409 = CARTESIAN_POINT ( 'NONE',  ( -1.500346250137462226E-14, 60.00000000000001421, -3.000000000000000000 ) ) ;
#9410 = CARTESIAN_POINT ( 'NONE',  ( 10.00000000000000000, 60.65655256511316651, -59.63197188857461128 ) ) ;
#9411 = EDGE_CURVE ( 'NONE', #14552, #1054, #21735, .T. ) ;
#9412 = FACE_OUTER_BOUND ( 'NONE', #21826, .T. ) ;
#9413 = CARTESIAN_POINT ( 'NONE',  ( 5.000000000000002665, 18.94217447942559573, 85.93715160505956874 ) ) ;
#9414 = CARTESIAN_POINT ( 'NONE',  ( 10.00000000000000000, 0.000000000000000000, 0.000000000000000000 ) ) ;
#9415 = AXIS2_PLACEMENT_3D ( 'NONE', #19326, #14132, #9368 ) ;
#9416 = AXIS2_PLACEMENT_3D ( 'NONE', #10554, #68, #20722 ) ;
#9417 = ORIENTED_EDGE ( 'NONE', *, *, #2439, .T. ) ;
#9418 = CIRCLE ( 'NONE', #12610, 44.99999999999999289 ) ;
#9419 = DIRECTION ( 'NONE',  ( -1.000000000000000000, 0.000000000000000000, 0.000000000000000000 ) ) ;
#9420 = ORIENTED_EDGE ( 'NONE', *, *, #9740, .F. ) ;
#9421 = CYLINDRICAL_SURFACE ( 'NONE', #4502, 44.99999999999999289 ) ;
#9422 = DIRECTION ( 'NONE',  ( -1.000000000000000000, -0.000000000000000000, 0.000000000000000000 ) ) ;
#9423 = CARTESIAN_POINT ( 'NONE',  ( 10.00000000000000000, 28.15804365424197186, -1.358152127006073684 ) ) ;
#9424 = VERTEX_POINT ( 'NONE', #12900 ) ;
#9425 = SURFACE_STYLE_FILL_AREA ( #12751 ) ;
#9426 = ORIENTED_EDGE ( 'NONE', *, *, #8271, .F. ) ;
#9427 = ORIENTED_EDGE ( 'NONE', *, *, #8381, .T. ) ;
#9428 = EDGE_CURVE ( 'NONE', #13513, #910, #19649, .T. ) ;
#9429 = AXIS2_PLACEMENT_3D ( 'NONE', #5158, #10327, #13542 ) ;
#9430 = EDGE_CURVE ( 'NONE', #12184, #8096, #4515, .T. ) ;
#9431 = ORIENTED_EDGE ( 'NONE', *, *, #4866, .F. ) ;
#9432 = CIRCLE ( 'NONE', #15804, 44.99999999999998579 ) ;
#9433 = EDGE_CURVE ( 'NONE', #8720, #14473, #18881, .T. ) ;
#9434 = CARTESIAN_POINT ( 'NONE',  ( 10.00000000000000000, -9.646732466564730046, -84.51112348751858860 ) ) ;
#9435 = CYLINDRICAL_SURFACE ( 'NONE', #5918, 32.00000000000000000 ) ;
#9436 = ORIENTED_EDGE ( 'NONE', *, *, #1086, .F. ) ;
#9437 = EDGE_CURVE ( 'NONE', #2378, #16156, #4775, .T. ) ;
#9438 = CARTESIAN_POINT ( 'NONE',  ( 10.00000000000000000, -29.47587714450981622, -82.91666097089152743 ) ) ;
#9439 = CYLINDRICAL_SURFACE ( 'NONE', #293, 88.00000000000000000 ) ;
#9440 = DIRECTION ( 'NONE',  ( 0.000000000000000000, 0.7431448254773910245, 0.6691306063588617903 ) ) ;
#9441 = DIRECTION ( 'NONE',  ( 1.000000000000000000, 0.000000000000000000, 0.000000000000000000 ) ) ;
#9442 = DIRECTION ( 'NONE',  ( -1.000000000000000000, -0.000000000000000000, 0.000000000000000000 ) ) ;
#9443 = VERTEX_POINT ( 'NONE', #11250 ) ;
#9444 = CARTESIAN_POINT ( 'NONE',  ( 0.000000000000000000, 27.87320266523557777, 88.20158487341770126 ) ) ;
#9445 = ADVANCED_FACE ( 'NONE', ( #16322 ), #10016, .F. ) ;
#9446 = CIRCLE ( 'NONE', #16164, 92.50100000000000477 ) ;
#9447 = AXIS2_PLACEMENT_3D ( 'NONE', #21033, #9196, #19590 ) ;
#9448 = CARTESIAN_POINT ( 'NONE',  ( 10.00000000000000000, 35.34277389771534672, 85.48288328206398035 ) ) ;
#9449 = AXIS2_PLACEMENT_3D ( 'NONE', #4223, #14157, #9282 ) ;
#9450 = ORIENTED_EDGE ( 'NONE', *, *, #16482, .T. ) ;
#9451 = CIRCLE ( 'NONE', #3128, 44.99999999999999289 ) ;
#9452 = EDGE_CURVE ( 'NONE', #20371, #12792, #2955, .T. ) ;
#9453 = DIRECTION ( 'NONE',  ( 0.000000000000000000, 0.9993908270190958731, -0.03489949670249761771 ) ) ;
#9454 = ORIENTED_EDGE ( 'NONE', *, *, #2702, .T. ) ;
#9455 = LINE ( 'NONE', #8148, #15490 ) ;
#9456 = PLANE ( 'NONE',  #12316 ) ;
#9457 = VERTEX_POINT ( 'NONE', #3286 ) ;
#9458 = CARTESIAN_POINT ( 'NONE',  ( 5.000000000000000888, 31.75612719289740937, 3.943144139962659445 ) ) ;
#9459 = ORIENTED_EDGE ( 'NONE', *, *, #11657, .T. ) ;
#9460 = ORIENTED_EDGE ( 'NONE', *, *, #524, .F. ) ;
#9461 = VERTEX_POINT ( 'NONE', #8051 ) ;
#9462 = EDGE_CURVE ( 'NONE', #1449, #18403, #14291, .T. ) ;
#9463 = DIRECTION ( 'NONE',  ( 1.000000000000000000, 0.000000000000000000, 0.000000000000000000 ) ) ;
#9464 = ORIENTED_EDGE ( 'NONE', *, *, #9987, .T. ) ;
#9465 = CARTESIAN_POINT ( 'NONE',  ( 10.00000000000000000, 0.000000000000000000, 0.000000000000000000 ) ) ;
#9466 = AXIS2_PLACEMENT_3D ( 'NONE', #20760, #5198, #17007 ) ;
#9467 = EDGE_CURVE ( 'NONE', #3479, #17932, #8160, .T. ) ;
#9468 = DIRECTION ( 'NONE',  ( 0.000000000000000000, 0.000000000000000000, 1.000000000000000000 ) ) ;
#9469 = CARTESIAN_POINT ( 'NONE',  ( 10.00000000000000000, 6.797690662956386021, -87.73705831432209834 ) ) ;
#9470 = AXIS2_PLACEMENT_3D ( 'NONE', #12029, #3624, #10357 ) ;
#9471 = CIRCLE ( 'NONE', #20443, 103.6249999999999716 ) ;
#9472 = VECTOR ( 'NONE', #1929, 1000.000000000000000 ) ;
#9473 = AXIS2_PLACEMENT_3D ( 'NONE', #5206, #15350, #3543 ) ;
#9474 = CYLINDRICAL_SURFACE ( 'NONE', #2233, 7.500000000000020428 ) ;
#9475 = DIRECTION ( 'NONE',  ( 1.000000000000000000, 0.000000000000000000, 0.000000000000000000 ) ) ;
#9476 = DIRECTION ( 'NONE',  ( 0.000000000000000000, -0.6427876096865300370, -0.7660444431189857850 ) ) ;
#9477 = DIRECTION ( 'NONE',  ( 1.000000000000000000, 0.000000000000000000, 0.000000000000000000 ) ) ;
#9478 = DIRECTION ( 'NONE',  ( 0.000000000000000000, 0.000000000000000000, -1.000000000000000000 ) ) ;
#9479 = EDGE_CURVE ( 'NONE', #8452, #6908, #15348, .T. ) ;
#9480 = EDGE_CURVE ( 'NONE', #16476, #21544, #7600, .T. ) ;
#9481 = CARTESIAN_POINT ( 'NONE',  ( -10.00000000000000000, 0.000000000000000000, 0.000000000000000000 ) ) ;
#9482 = AXIS2_PLACEMENT_3D ( 'NONE', #15100, #13115, #16654 ) ;
#9483 = ORIENTED_EDGE ( 'NONE', *, *, #1217, .F. ) ;
#9484 = AXIS2_PLACEMENT_3D ( 'NONE', #14660, #13002, #12562 ) ;
#9485 = ORIENTED_EDGE ( 'NONE', *, *, #6527, .T. ) ;
#9486 = EDGE_CURVE ( 'NONE', #13543, #15275, #19948, .T. ) ;
#9487 = AXIS2_PLACEMENT_3D ( 'NONE', #841, #3845, #10579 ) ;
#9488 = EDGE_CURVE ( 'NONE', #5595, #11274, #9348, .T. ) ;
#9489 = ORIENTED_EDGE ( 'NONE', *, *, #13068, .T. ) ;
#9490 = ORIENTED_EDGE ( 'NONE', *, *, #19998, .F. ) ;
#9491 = EDGE_LOOP ( 'NONE', ( #7460, #20614, #13268, #17883 ) ) ;
#9492 = DIRECTION ( 'NONE',  ( 0.000000000000000000, 0.000000000000000000, 1.000000000000000000 ) ) ;
#9493 = EDGE_CURVE ( 'NONE', #11265, #7508, #21711, .T. ) ;
#9494 = ORIENTED_EDGE ( 'NONE', *, *, #1993, .F. ) ;
#9495 = FACE_OUTER_BOUND ( 'NONE', #17817, .T. ) ;
#9496 = DIRECTION ( 'NONE',  ( 0.000000000000000000, -0.2079116908177468248, -0.9781476007338083534 ) ) ;
#9497 = CIRCLE ( 'NONE', #20804, 88.00000000000000000 ) ;
#9498 = CARTESIAN_POINT ( 'NONE',  ( 10.00000000000000000, 0.000000000000000000, 32.00000000000000000 ) ) ;
#9499 = CARTESIAN_POINT ( 'NONE',  ( 5.000000000000002665, -35.18804927320473297, -80.65854690202716881 ) ) ;
#9500 = FACE_OUTER_BOUND ( 'NONE', #6968, .T. ) ;
#9501 = AXIS2_PLACEMENT_3D ( 'NONE', #19040, #7333, #18721 ) ;
#9502 = AXIS2_PLACEMENT_3D ( 'NONE', #21398, #16091, #11230 ) ;
#9503 = CARTESIAN_POINT ( 'NONE',  ( 10.00000000000000000, -84.19736439813780748, -38.30455363801015523 ) ) ;
#9504 = DIRECTION ( 'NONE',  ( -1.000000000000000000, -0.000000000000000000, -0.000000000000000000 ) ) ;
#9505 = LINE ( 'NONE', #13259, #317 ) ;
#9506 = ORIENTED_EDGE ( 'NONE', *, *, #15582, .T. ) ;
#9507 = CARTESIAN_POINT ( 'NONE',  ( 10.00000000000000000, -56.34908017029602689, 63.71789861856433390 ) ) ;
#9508 = EDGE_LOOP ( 'NONE', ( #15360, #6794, #9551, #17548 ) ) ;
#9509 = EDGE_CURVE ( 'NONE', #5155, #18369, #10409, .T. ) ;
#9510 = CYLINDRICAL_SURFACE ( 'NONE', #5245, 44.99999999999999289 ) ;
#9511 = DIRECTION ( 'NONE',  ( -1.000000000000000000, -0.000000000000000000, -0.000000000000000000 ) ) ;
#9512 = ORIENTED_EDGE ( 'NONE', *, *, #19701, .F. ) ;
#9513 = CIRCLE ( 'NONE', #14467, 44.99999999999999289 ) ;
#9514 = DIRECTION ( 'NONE',  ( -1.000000000000000000, -0.000000000000000000, -0.000000000000000000 ) ) ;
#9515 = EDGE_LOOP ( 'NONE', ( #20442, #18024, #11219, #15637 ) ) ;
#9516 = ORIENTED_EDGE ( 'NONE', *, *, #9708, .T. ) ;
#9517 =( LENGTH_UNIT ( ) NAMED_UNIT ( * ) SI_UNIT ( .MILLI., .METRE. ) );
#9518 = DIRECTION ( 'NONE',  ( 0.000000000000000000, 0.000000000000000000, 1.000000000000000000 ) ) ;
#9519 = EDGE_LOOP ( 'NONE', ( #4368, #18235, #529, #1735 ) ) ;
#9520 = VERTEX_POINT ( 'NONE', #13557 ) ;
#9521 = CARTESIAN_POINT ( 'NONE',  ( 10.00000000000000000, -6.797690662955810481, 87.73705831432212676 ) ) ;
#9522 = CARTESIAN_POINT ( 'NONE',  ( 0.000000000000000000, 0.000000000000000000, 3.000000000000000000 ) ) ;
#9523 = CARTESIAN_POINT ( 'NONE',  ( -140.0000507999999968, 0.000000000000000000, 0.000000000000000000 ) ) ;
#9524 = CARTESIAN_POINT ( 'NONE',  ( 10.00000000000000000, -52.34334029047821701, -76.26670130689538496 ) ) ;
#9525 = DIRECTION ( 'NONE',  ( -1.000000000000000000, 0.000000000000000000, -0.000000000000000000 ) ) ;
#9526 = DIRECTION ( 'NONE',  ( 0.000000000000000000, 0.000000000000000000, 1.000000000000000000 ) ) ;
#9527 = CARTESIAN_POINT ( 'NONE',  ( 0.000000000000000000, -12.90135963484139658, 87.04915231966639055 ) ) ;
#9528 = CARTESIAN_POINT ( 'NONE',  ( 10.00000000000000000, 0.000000000000000000, 0.000000000000000000 ) ) ;
#9529 = DIRECTION ( 'NONE',  ( 0.000000000000000000, 0.000000000000000000, 1.000000000000000000 ) ) ;
#9530 = EDGE_LOOP ( 'NONE', ( #9697, #17148, #19634, #18900 ) ) ;
#9531 = CARTESIAN_POINT ( 'NONE',  ( 10.00000000000000000, 30.24235385705238244, 10.45944707835118059 ) ) ;
#9532 = ADVANCED_FACE ( 'NONE', ( #3606 ), #5379, .F. ) ;
#9533 = ORIENTED_EDGE ( 'NONE', *, *, #9889, .T. ) ;
#9534 = CARTESIAN_POINT ( 'NONE',  ( 10.00000000000000000, -12.90135963484139658, 87.04915231966639055 ) ) ;
#9535 = DIRECTION ( 'NONE',  ( 1.000000000000000000, 0.000000000000000000, 0.000000000000000000 ) ) ;
#9536 = FACE_OUTER_BOUND ( 'NONE', #6853, .T. ) ;
#9537 = ORIENTED_EDGE ( 'NONE', *, *, #3767, .F. ) ;
#9538 = EDGE_CURVE ( 'NONE', #17965, #20371, #18192, .T. ) ;
#9539 = ORIENTED_EDGE ( 'NONE', *, *, #4618, .F. ) ;
#9540 = ORIENTED_EDGE ( 'NONE', *, *, #8153, .F. ) ;
#9541 = EDGE_LOOP ( 'NONE', ( #2365, #12757, #10661, #14975 ) ) ;
#9542 = AXIS2_PLACEMENT_3D ( 'NONE', #21616, #16315, #4614 ) ;
#9543 = DIRECTION ( 'NONE',  ( 0.000000000000000000, 0.000000000000000000, -1.000000000000000000 ) ) ;
#9544 = CARTESIAN_POINT ( 'NONE',  ( 0.000000000000000000, 0.000000000000000000, 0.000000000000000000 ) ) ;
#9545 = ORIENTED_EDGE ( 'NONE', *, *, #2317, .T. ) ;
#9546 = DIRECTION ( 'NONE',  ( 1.000000000000000000, -0.000000000000000000, 0.000000000000000000 ) ) ;
#9547 = CARTESIAN_POINT ( 'NONE',  ( 10.00000000000000000, -70.37753541435978377, 60.02863908169610596 ) ) ;
#9548 = CARTESIAN_POINT ( 'NONE',  ( 10.00000000000000000, -30.71797041605752554, -82.46457599186584275 ) ) ;
#9549 = CARTESIAN_POINT ( 'NONE',  ( 10.00000000000000000, 26.69209308833507777, 6.612652082459410607 ) ) ;
#9550 = DIRECTION ( 'NONE',  ( 0.000000000000000000, 0.000000000000000000, -1.000000000000000000 ) ) ;
#9551 = ORIENTED_EDGE ( 'NONE', *, *, #17320, .T. ) ;
#9552 = CARTESIAN_POINT ( 'NONE',  ( 10.00000000000000000, 73.32282170386848463, 48.65967342042804944 ) ) ;
#9553 = CARTESIAN_POINT ( 'NONE',  ( 0.000000000000000000, 19.85071254963777676, 20.01672328094538145 ) ) ;
#9554 = ADVANCED_FACE ( 'NONE', ( #196 ), #3508, .F. ) ;
#9555 = ORIENTED_EDGE ( 'NONE', *, *, #21365, .F. ) ;
#9556 = DIRECTION ( 'NONE',  ( 1.000000000000000000, 0.000000000000000000, -0.000000000000000000 ) ) ;
#9557 = VERTEX_POINT ( 'NONE', #1845 ) ;
#9558 = CYLINDRICAL_SURFACE ( 'NONE', #11617, 88.00000000000000000 ) ;
#9559 = FACE_OUTER_BOUND ( 'NONE', #9519, .T. ) ;
#9560 = ORIENTED_EDGE ( 'NONE', *, *, #10813, .F. ) ;
#9561 = DIRECTION ( 'NONE',  ( 0.000000000000000000, 0.000000000000000000, -1.000000000000000000 ) ) ;
#9562 = VERTEX_POINT ( 'NONE', #5280 ) ;
#9563 = VERTEX_POINT ( 'NONE', #8806 ) ;
#9564 = CARTESIAN_POINT ( 'NONE',  ( -1.500000000000000000, 15.00000000000000000, 7.000000000000000000 ) ) ;
#9565 = EDGE_LOOP ( 'NONE', ( #398, #1497, #17657, #9586 ) ) ;
#9566 = EDGE_CURVE ( 'NONE', #1295, #16815, #1206, .T. ) ;
#9567 = CARTESIAN_POINT ( 'NONE',  ( 0.000000000000000000, 24.17932380791746994, -20.96092317126981186 ) ) ;
#9568 = DIRECTION ( 'NONE',  ( -1.000000000000000000, 0.000000000000000000, -0.000000000000000000 ) ) ;
#9569 = CARTESIAN_POINT ( 'NONE',  ( 10.00000000000000000, -52.25832601289145884, 70.80301803122767978 ) ) ;
#9570 =( GEOMETRIC_REPRESENTATION_CONTEXT ( 3 ) GLOBAL_UNCERTAINTY_ASSIGNED_CONTEXT ( ( #5411 ) ) GLOBAL_UNIT_ASSIGNED_CONTEXT ( ( #2237, #17381, #8867 ) ) REPRESENTATION_CONTEXT ( 'NONE', 'WORKASPACE' ) );
#9571 = CARTESIAN_POINT ( 'NONE',  ( 10.49999999999999822, 1.285879139104720633E-15, 3.000000000000000000 ) ) ;
#9572 = CARTESIAN_POINT ( 'NONE',  ( 0.000000000000000000, 56.05743251323954013, -67.83483072893743326 ) ) ;
#9573 = CARTESIAN_POINT ( 'NONE',  ( -140.0000507999999968, 0.000000000000000000, 0.000000000000000000 ) ) ;
#9574 = CARTESIAN_POINT ( 'NONE',  ( 10.00000000000000000, 41.87002153499110335, 74.04114219178059386 ) ) ;
#9575 = DIRECTION ( 'NONE',  ( 0.000000000000000000, 0.000000000000000000, 1.000000000000000000 ) ) ;
#9576 = EDGE_CURVE ( 'NONE', #1586, #8180, #10028, .T. ) ;
#9577 = EDGE_CURVE ( 'NONE', #14952, #1865, #18653, .T. ) ;
#9578 = EDGE_CURVE ( 'NONE', #2563, #389, #12010, .T. ) ;
#9579 = CARTESIAN_POINT ( 'NONE',  ( 0.000000000000000000, -56.34908017029602689, 63.71789861856433390 ) ) ;
#9580 = ORIENTED_EDGE ( 'NONE', *, *, #4026, .T. ) ;
#9581 = EDGE_CURVE ( 'NONE', #10412, #19966, #6522, .T. ) ;
#9582 = ORIENTED_EDGE ( 'NONE', *, *, #7342, .T. ) ;
#9583 = ORIENTED_EDGE ( 'NONE', *, *, #4484, .T. ) ;
#9584 = EDGE_CURVE ( 'NONE', #13159, #1625, #1956, .T. ) ;
#9585 = AXIS2_PLACEMENT_3D ( 'NONE', #19026, #3660, #15591 ) ;
#9586 = ORIENTED_EDGE ( 'NONE', *, *, #4967, .T. ) ;
#9587 = ORIENTED_EDGE ( 'NONE', *, *, #21199, .F. ) ;
#9588 = ADVANCED_FACE ( 'NONE', ( #305 ), #405, .F. ) ;
#9589 = CYLINDRICAL_SURFACE ( 'NONE', #18313, 88.00000000000000000 ) ;
#9590 = CIRCLE ( 'NONE', #5739, 5.000000000000000000 ) ;
#9591 = ORIENTED_EDGE ( 'NONE', *, *, #4349, .T. ) ;
#9592 = CARTESIAN_POINT ( 'NONE',  ( 1.399999999999998579, 0.000000000000000000, 0.000000000000000000 ) ) ;
#9593 = CARTESIAN_POINT ( 'NONE',  ( 0.000000000000000000, -85.22372865846278955, -21.92979875759713693 ) ) ;
#9594 = EDGE_CURVE ( 'NONE', #20730, #21817, #7558, .T. ) ;
#9595 = DIRECTION ( 'NONE',  ( -1.000000000000000000, -0.000000000000000000, -0.000000000000000000 ) ) ;
#9596 = CYLINDRICAL_SURFACE ( 'NONE', #10531, 11.99999999999999822 ) ;
#9597 = PLANE ( 'NONE',  #15409 ) ;
#9598 = EDGE_CURVE ( 'NONE', #6056, #13893, #16878, .T. ) ;
#9599 = DIRECTION ( 'NONE',  ( 0.000000000000000000, 0.000000000000000000, -1.000000000000000000 ) ) ;
#9600 = DIRECTION ( 'NONE',  ( -1.000000000000000000, -0.000000000000000000, -0.000000000000000000 ) ) ;
#9601 = COLOUR_RGB ( '', 0.66274510, 0.83137255, 0.94901961) ;
#9602 = ORIENTED_EDGE ( 'NONE', *, *, #1666, .F. ) ;
#9603 = CYLINDRICAL_SURFACE ( 'NONE', #21719, 12.00000000000000000 ) ;
#9604 = AXIS2_PLACEMENT_3D ( 'NONE', #14915, #18461, #1770 ) ;
#9605 = ADVANCED_FACE ( 'NONE', ( #15543 ), #7143, .F. ) ;
#9606 = VERTEX_POINT ( 'NONE', #9122 ) ;
#9607 = CIRCLE ( 'NONE', #9982, 92.50100000000000477 ) ;
#9608 = VERTEX_POINT ( 'NONE', #19079 ) ;
#9609 = DIRECTION ( 'NONE',  ( 1.000000000000000000, -0.000000000000000000, -0.000000000000000000 ) ) ;
#9610 = DIRECTION ( 'NONE',  ( 1.000000000000000000, 0.000000000000000000, 0.000000000000000000 ) ) ;
#9611 = VERTEX_POINT ( 'NONE', #12652 ) ;
#9612 = CARTESIAN_POINT ( 'NONE',  ( 10.00000000000000000, -75.27139873020921357, 53.76477968147791131 ) ) ;
#9613 = ORIENTED_EDGE ( 'NONE', *, *, #17427, .F. ) ;
#9614 = ORIENTED_EDGE ( 'NONE', *, *, #20020, .F. ) ;
#9615 = SHAPE_DEFINITION_REPRESENTATION ( #17096, #4577 ) ;
#9616 = DIRECTION ( 'NONE',  ( -1.000000000000000000, -0.000000000000000000, 0.000000000000000000 ) ) ;
#9617 = VECTOR ( 'NONE', #13019, 1000.000000000000000 ) ;
#9618 = ORIENTED_EDGE ( 'NONE', *, *, #6548, .T. ) ;
#9619 = ORIENTED_EDGE ( 'NONE', *, *, #6750, .F. ) ;
#9620 = DIRECTION ( 'NONE',  ( 0.000000000000000000, 0.000000000000000000, -1.000000000000000000 ) ) ;
#9621 = EDGE_CURVE ( 'NONE', #14609, #18291, #3675, .T. ) ;
#9622 = CARTESIAN_POINT ( 'NONE',  ( 10.00000000000000000, 85.05652083079336023, -0.7600687895862878740 ) ) ;
#9623 = AXIS2_PLACEMENT_3D ( 'NONE', #3484, #13757, #2148 ) ;
#9624 = AXIS2_PLACEMENT_3D ( 'NONE', #19762, #4285, #19530 ) ;
#9625 = DIRECTION ( 'NONE',  ( 0.000000000000000000, 0.000000000000000000, 1.000000000000000000 ) ) ;
#9626 = CARTESIAN_POINT ( 'NONE',  ( 0.000000000000000000, -7.409634587003275819, 27.19958299168154880 ) ) ;
#9627 = CARTESIAN_POINT ( 'NONE',  ( 0.000000000000000000, -61.33825423015729683, 69.23910433415923649 ) ) ;
#9628 = EDGE_CURVE ( 'NONE', #15096, #10277, #14314, .T. ) ;
#9629 = FACE_OUTER_BOUND ( 'NONE', #15937, .T. ) ;
#9630 = AXIS2_PLACEMENT_3D ( 'NONE', #15638, #14196, #9326 ) ;
#9631 = EDGE_CURVE ( 'NONE', #7099, #19664, #9659, .T. ) ;
#9632 = CYLINDRICAL_SURFACE ( 'NONE', #11420, 5.000000000000000000 ) ;
#9633 = CARTESIAN_POINT ( 'NONE',  ( 10.00000000000000000, -43.18649929580143976, -73.28107340219457910 ) ) ;
#9634 = DIRECTION ( 'NONE',  ( -1.000000000000000000, -0.000000000000000000, -0.000000000000000000 ) ) ;
#9635 = ORIENTED_EDGE ( 'NONE', *, *, #7613, .F. ) ;
#9636 = VECTOR ( 'NONE', #10246, 1000.000000000000000 ) ;
#9637 = ORIENTED_EDGE ( 'NONE', *, *, #12026, .T. ) ;
#9638 = DIRECTION ( 'NONE',  ( -1.000000000000000000, -0.000000000000000000, -0.000000000000000000 ) ) ;
#9639 = AXIS2_PLACEMENT_3D ( 'NONE', #10295, #1901, #13730 ) ;
#9640 = CARTESIAN_POINT ( 'NONE',  ( 0.000000000000000000, -3.974475837764314345, -92.41557521768193340 ) ) ;
#9641 = DIRECTION ( 'NONE',  ( -1.000000000000000000, -0.000000000000000000, -0.000000000000000000 ) ) ;
#9642 = PRODUCT ( 'instrument roller bearing_iso_ISO 1224 - 171015 - R,24,SI,NC,24', 'instrument roller bearing_iso_ISO 1224 - 171015 - R,24,SI,NC,24', '', ( #12832 ) ) ;
#9643 = ORIENTED_EDGE ( 'NONE', *, *, #16125, .F. ) ;
#9644 = AXIS2_PLACEMENT_3D ( 'NONE', #9434, #16191, #1057 ) ;
#9645 = EDGE_LOOP ( 'NONE', ( #5045, #1323, #5566, #1150 ) ) ;
#9646 = EDGE_LOOP ( 'NONE', ( #7984, #15599, #9635, #11243 ) ) ;
#9647 = ORIENTED_EDGE ( 'NONE', *, *, #17576, .T. ) ;
#9648 = FACE_OUTER_BOUND ( 'NONE', #15203, .T. ) ;
#9649 = CARTESIAN_POINT ( 'NONE',  ( 0.000000000000000000, 83.48638250753229784, 27.82128566055142826 ) ) ;
#9650 = EDGE_LOOP ( 'NONE', ( #7410, #13749, #5478, #8522 ) ) ;
#9651 = AXIS2_PLACEMENT_3D ( 'NONE', #7781, #20820, #19153 ) ;
#9652 = FACE_BOUND ( 'NONE', #15122, .T. ) ;
#9653 = LINE ( 'NONE', #6378, #7649 ) ;
#9654 = CARTESIAN_POINT ( 'NONE',  ( 0.000000000000000000, 0.000000000000000000, 0.000000000000000000 ) ) ;
#9655 = CARTESIAN_POINT ( 'NONE',  ( 0.000000000000000000, -64.95266917914277371, -59.37298010463037912 ) ) ;
#9656 = DIRECTION ( 'NONE',  ( 0.000000000000000000, 0.000000000000000000, 1.000000000000000000 ) ) ;
#9657 = CARTESIAN_POINT ( 'NONE',  ( 10.00000000000000000, 0.000000000000000000, 0.000000000000000000 ) ) ;
#9658 = UNCERTAINTY_MEASURE_WITH_UNIT (LENGTH_MEASURE( 1.000000000000000082E-05 ), #10091, 'distance_accuracy_value', 'NONE');
#9659 = CIRCLE ( 'NONE', #511, 92.50100000000000477 ) ;
#9660 = ORIENTED_EDGE ( 'NONE', *, *, #1052, .T. ) ;
#9661 = VECTOR ( 'NONE', #21573, 1000.000000000000000 ) ;
#9662 = DIRECTION ( 'NONE',  ( -0.000000000000000000, 0.000000000000000000, 1.000000000000000000 ) ) ;
#9663 = FACE_OUTER_BOUND ( 'NONE', #10326, .T. ) ;
#9664 = VERTEX_POINT ( 'NONE', #17417 ) ;
#9665 = LINE ( 'NONE', #16744, #2714 ) ;
#9666 = ORIENTED_EDGE ( 'NONE', *, *, #21107, .F. ) ;
#9667 = VECTOR ( 'NONE', #17016, 1000.000000000000000 ) ;
#9668 = DIRECTION ( 'NONE',  ( 0.000000000000000000, 0.000000000000000000, 1.000000000000000000 ) ) ;
#9669 = AXIS2_PLACEMENT_3D ( 'NONE', #18955, #3699, #14083 ) ;
#9670 = CARTESIAN_POINT ( 'NONE',  ( 10.00000000000000000, -68.36541360927220978, 50.60987712331682076 ) ) ;
#9671 = VERTEX_POINT ( 'NONE', #734 ) ;
#9672 = CARTESIAN_POINT ( 'NONE',  ( -1.500000000000000000, 100.0000000000000000, 4.769696007084728073 ) ) ;
#9673 = AXIS2_PLACEMENT_3D ( 'NONE', #8133, #6479, #4812 ) ;
#9674 = ORIENTED_EDGE ( 'NONE', *, *, #4468, .T. ) ;
#9675 = ORIENTED_EDGE ( 'NONE', *, *, #9915, .F. ) ;
#9676 = CARTESIAN_POINT ( 'NONE',  ( 0.000000000000000000, -24.89070495400676819, -84.40647372620527733 ) ) ;
#9677 = VECTOR ( 'NONE', #19049, 1000.000000000000000 ) ;
#9678 = ORIENTED_EDGE ( 'NONE', *, *, #1624, .T. ) ;
#9679 = DIRECTION ( 'NONE',  ( 0.000000000000000000, 0.000000000000000000, -1.000000000000000000 ) ) ;
#9680 = CARTESIAN_POINT ( 'NONE',  ( 10.00000000000000000, 9.366510754379232750, 25.85466064925429208 ) ) ;
#9681 = CARTESIAN_POINT ( 'NONE',  ( 10.00000000000000000, 69.25892805976512534, 49.38005998797868301 ) ) ;
#9682 = ADVANCED_FACE ( 'NONE', ( #7472 ), #12334, .F. ) ;
#9683 = DIRECTION ( 'NONE',  ( 1.000000000000000000, 0.000000000000000000, 0.000000000000000000 ) ) ;
#9684 = CIRCLE ( 'NONE', #181, 92.50100000000003320 ) ;
#9685 = DIRECTION ( 'NONE',  ( 0.000000000000000000, 0.000000000000000000, 1.000000000000000000 ) ) ;
#9686 = CARTESIAN_POINT ( 'NONE',  ( 10.00000000000000000, 0.000000000000000000, 0.000000000000000000 ) ) ;
#9687 = EDGE_CURVE ( 'NONE', #453, #215, #2168, .T. ) ;
#9688 = CIRCLE ( 'NONE', #6912, 44.99999999999999289 ) ;
#9689 = CARTESIAN_POINT ( 'NONE',  ( 0.000000000000000000, 0.000000000000000000, 0.000000000000000000 ) ) ;
#9690 = DIRECTION ( 'NONE',  ( 0.000000000000000000, 0.000000000000000000, -1.000000000000000000 ) ) ;
#9691 = CARTESIAN_POINT ( 'NONE',  ( 10.00000000000000000, -28.15804365424197897, 1.358152127005888055 ) ) ;
#9692 = CIRCLE ( 'NONE', #4758, 44.99999999999999289 ) ;
#9693 = DIRECTION ( 'NONE',  ( 0.000000000000000000, 0.000000000000000000, 1.000000000000000000 ) ) ;
#9694 = ORIENTED_EDGE ( 'NONE', *, *, #19219, .T. ) ;
#9695 = ORIENTED_EDGE ( 'NONE', *, *, #17755, .F. ) ;
#9696 = VERTEX_POINT ( 'NONE', #14201 ) ;
#9697 = ORIENTED_EDGE ( 'NONE', *, *, #3982, .F. ) ;
#9698 = CIRCLE ( 'NONE', #12531, 44.99999999999999289 ) ;
#9699 = AXIS2_PLACEMENT_3D ( 'NONE', #4801, #8010, #13077 ) ;
#9700 = AXIS2_PLACEMENT_3D ( 'NONE', #15103, #21849, #6736 ) ;
#9701 = VERTEX_POINT ( 'NONE', #21172 ) ;
#9702 = CIRCLE ( 'NONE', #15361, 44.99999999999998579 ) ;
#9703 = CARTESIAN_POINT ( 'NONE',  ( 10.00000000000000000, -77.39385041987173963, 35.28996114464576550 ) ) ;
#9704 = ORIENTED_EDGE ( 'NONE', *, *, #14050, .T. ) ;
#9705 = CARTESIAN_POINT ( 'NONE',  ( -90.00000000000000000, 6.123233995736767268E-16, 5.000000000000000888 ) ) ;
#9706 = EDGE_CURVE ( 'NONE', #5372, #18348, #20948, .T. ) ;
#9707 = EDGE_CURVE ( 'NONE', #3550, #7280, #19911, .T. ) ;
#9708 = EDGE_CURVE ( 'NONE', #2019, #5209, #15641, .T. ) ;
#9709 = DIRECTION ( 'NONE',  ( -1.000000000000000000, -0.000000000000000000, -0.000000000000000000 ) ) ;
#9710 = EDGE_CURVE ( 'NONE', #19677, #6016, #10999, .T. ) ;
#9711 = CARTESIAN_POINT ( 'NONE',  ( 10.00000000000000000, 81.34229909304724515, -33.57723005635285318 ) ) ;
#9712 = CARTESIAN_POINT ( 'NONE',  ( 10.00000000000000000, -32.56745702629687855, -78.57830605990686479 ) ) ;
#9713 = CARTESIAN_POINT ( 'NONE',  ( 0.000000000000000000, 23.62010150527222052, 84.77081340225913664 ) ) ;
#9714 = CIRCLE ( 'NONE', #4087, 11.99999999999999467 ) ;
#9715 = FACE_OUTER_BOUND ( 'NONE', #6464, .T. ) ;
#9716 = CYLINDRICAL_SURFACE ( 'NONE', #14056, 88.00000000000000000 ) ;
#9717 = CIRCLE ( 'NONE', #17503, 92.50100000000000477 ) ;
#9718 = ORIENTED_EDGE ( 'NONE', *, *, #3505, .T. ) ;
#9719 = CIRCLE ( 'NONE', #4033, 92.50099999999999056 ) ;
#9720 = AXIS2_PLACEMENT_3D ( 'NONE', #10749, #19378, #7346 ) ;
#9721 = CARTESIAN_POINT ( 'NONE',  ( -10.00000000000000000, 0.000000000000000000, 0.000000000000000000 ) ) ;
#9722 = EDGE_CURVE ( 'NONE', #17553, #4799, #7260, .T. ) ;
#9723 = VECTOR ( 'NONE', #14122, 1000.000000000000000 ) ;
#9724 = VERTEX_POINT ( 'NONE', #4040 ) ;
#9725 = ORIENTED_EDGE ( 'NONE', *, *, #7136, .T. ) ;
#9726 = EDGE_CURVE ( 'NONE', #1128, #18258, #4156, .T. ) ;
#9727 = DIRECTION ( 'NONE',  ( 0.000000000000000000, 0.000000000000000000, 1.000000000000000000 ) ) ;
#9728 = ORIENTED_EDGE ( 'NONE', *, *, #3784, .T. ) ;
#9729 = DIRECTION ( 'NONE',  ( 1.000000000000000000, 0.000000000000000000, 0.000000000000000000 ) ) ;
#9730 = ORIENTED_EDGE ( 'NONE', *, *, #12972, .F. ) ;
#9731 = VERTEX_POINT ( 'NONE', #10889 ) ;
#9732 = DIRECTION ( 'NONE',  ( 0.000000000000000000, 1.000000000000000000, 0.000000000000000000 ) ) ;
#9733 = DIRECTION ( 'NONE',  ( 0.000000000000000000, 0.000000000000000000, -1.000000000000000000 ) ) ;
#9734 = VERTEX_POINT ( 'NONE', #19180 ) ;
#9735 = CIRCLE ( 'NONE', #7283, 7.400000000000020783 ) ;
#9736 = DIRECTION ( 'NONE',  ( 0.000000000000000000, -0.2079116908177666145, 0.9781476007338040235 ) ) ;
#9737 = CIRCLE ( 'NONE', #11864, 45.00000000000000000 ) ;
#9738 = DIRECTION ( 'NONE',  ( 0.000000000000000000, 0.000000000000000000, 1.000000000000000000 ) ) ;
#9739 = CIRCLE ( 'NONE', #19994, 11.99999999999999822 ) ;
#9740 = EDGE_CURVE ( 'NONE', #15128, #18259, #21674, .T. ) ;
#9741 = FACE_OUTER_BOUND ( 'NONE', #20137, .T. ) ;
#9742 = CARTESIAN_POINT ( 'NONE',  ( 10.00000000000000000, 0.000000000000000000, 0.000000000000000000 ) ) ;
#9743 = CARTESIAN_POINT ( 'NONE',  ( 0.000000000000000000, 75.45728100697598961, 39.26051685139091063 ) ) ;
#9744 = FACE_OUTER_BOUND ( 'NONE', #3760, .T. ) ;
#9745 = DIRECTION ( 'NONE',  ( 1.000000000000000000, -0.000000000000000000, -0.000000000000000000 ) ) ;
#9746 = CARTESIAN_POINT ( 'NONE',  ( 10.00000000000000000, 52.96496548042942010, -66.55750800669305534 ) ) ;
#9747 = DIRECTION ( 'NONE',  ( 0.000000000000000000, -0.4067366430758070917, 0.9135454576425978690 ) ) ;
#9748 = EDGE_LOOP ( 'NONE', ( #16670, #11074 ) ) ;
#9749 = EDGE_CURVE ( 'NONE', #20733, #19144, #5602, .T. ) ;
#9750 = ORIENTED_EDGE ( 'NONE', *, *, #8628, .F. ) ;
#9751 = CIRCLE ( 'NONE', #8006, 6.728125000000023448 ) ;
#9752 = ADVANCED_FACE ( 'NONE', ( #9222 ), #6862, .T. ) ;
#9753 = AXIS2_PLACEMENT_3D ( 'NONE', #21554, #19891, #7963 ) ;
#9754 = DIRECTION ( 'NONE',  ( -1.000000000000000000, 0.000000000000000000, 0.000000000000000000 ) ) ;
#9755 = DIRECTION ( 'NONE',  ( 0.000000000000000000, 0.7880107536067233465, -0.6156614753256567374 ) ) ;
#9756 = ORIENTED_EDGE ( 'NONE', *, *, #9621, .T. ) ;
#9757 = EDGE_CURVE ( 'NONE', #13772, #7164, #17440, .T. ) ;
#9758 = CARTESIAN_POINT ( 'NONE',  ( 0.000000000000000000, 92.22057093985031884, 7.197311757040840696 ) ) ;
#9759 = ORIENTED_EDGE ( 'NONE', *, *, #11380, .F. ) ;
#9760 = EDGE_CURVE ( 'NONE', #879, #6607, #852, .T. ) ;
#9761 =( LENGTH_UNIT ( ) NAMED_UNIT ( * ) SI_UNIT ( .MILLI., .METRE. ) );
#9762 = ORIENTED_EDGE ( 'NONE', *, *, #8776, .F. ) ;
#9763 = ORIENTED_EDGE ( 'NONE', *, *, #20431, .F. ) ;
#9764 = ORIENTED_EDGE ( 'NONE', *, *, #15537, .F. ) ;
#9765 = DIRECTION ( 'NONE',  ( 0.000000000000000000, 0.000000000000000000, -1.000000000000000000 ) ) ;
#9766 = CARTESIAN_POINT ( 'NONE',  ( 10.00000000000000000, -4.294029059350045863, 27.86182539015965176 ) ) ;
#9767 = ORIENTED_EDGE ( 'NONE', *, *, #2307, .T. ) ;
#9768 = VECTOR ( 'NONE', #6860, 1000.000000000000000 ) ;
#9769 = DIRECTION ( 'NONE',  ( -1.000000000000000000, 0.000000000000000000, 0.000000000000000000 ) ) ;
#9770 = CARTESIAN_POINT ( 'NONE',  ( 10.00000000000000000, -85.05652083079337444, 0.7600687895857258791 ) ) ;
#9771 = AXIS2_PLACEMENT_3D ( 'NONE', #1728, #14976, #3269 ) ;
#9772 = CYLINDRICAL_SURFACE ( 'NONE', #12552, 92.50100000000000477 ) ;
#9773 = CARTESIAN_POINT ( 'NONE',  ( 1.114299999999999846, 0.000000000000000000, -5.633200000000004870 ) ) ;
#9774 = AXIS2_PLACEMENT_3D ( 'NONE', #12466, #10922, #438 ) ;
#9775 = CARTESIAN_POINT ( 'NONE',  ( 0.000000000000000000, 64.95266917914317162, 59.37298010462993858 ) ) ;
#9776 = CARTESIAN_POINT ( 'NONE',  ( -8.900000000000019895, 0.000000000000000000, 0.000000000000000000 ) ) ;
#9777 = ORIENTED_EDGE ( 'NONE', *, *, #9576, .T. ) ;
#9778 = CARTESIAN_POINT ( 'NONE',  ( 10.00000000000000000, 0.000000000000000000, 0.000000000000000000 ) ) ;
#9779 = CARTESIAN_POINT ( 'NONE',  ( 10.00000000000000000, 31.15801000616942673, -79.14775961996359399 ) ) ;
#9780 = VERTEX_POINT ( 'NONE', #7689 ) ;
#9781 = CARTESIAN_POINT ( 'NONE',  ( 10.00000000000000000, 17.83210509884640871, 21.83428559348767806 ) ) ;
#9782 = VERTEX_POINT ( 'NONE', #19504 ) ;
#9783 = VECTOR ( 'NONE', #9251, 1000.000000000000000 ) ;
#9784 = CARTESIAN_POINT ( 'NONE',  ( -10.00000000000000000, 0.000000000000000000, 0.000000000000000000 ) ) ;
#9785 = AXIS2_PLACEMENT_3D ( 'NONE', #20608, #15527, #2052 ) ;
#9786 = DIRECTION ( 'NONE',  ( 0.000000000000000000, -6.938893903907230744E-15, 1.000000000000000000 ) ) ;
#9787 = AXIS2_PLACEMENT_3D ( 'NONE', #4959, #13674, #1749 ) ;
#9788 = EDGE_LOOP ( 'NONE', ( #16803, #7309, #21641, #8315 ) ) ;
#9789 = FACE_OUTER_BOUND ( 'NONE', #6848, .T. ) ;
#9790 = EDGE_LOOP ( 'NONE', ( #10417, #1704 ) ) ;
#9791 = ORIENTED_EDGE ( 'NONE', *, *, #5662, .F. ) ;
#9792 = FACE_OUTER_BOUND ( 'NONE', #17931, .T. ) ;
#9793 = EDGE_LOOP ( 'NONE', ( #12854, #10363, #6855, #8248 ) ) ;
#9794 = DIRECTION ( 'NONE',  ( 0.000000000000000000, 0.000000000000000000, 1.000000000000000000 ) ) ;
#9795 = CARTESIAN_POINT ( 'NONE',  ( 10.00000000000000000, 0.000000000000000000, 0.000000000000000000 ) ) ;
#9796 = CARTESIAN_POINT ( 'NONE',  ( 5.000000000000002665, -30.71797041605864464, 82.46457599186540222 ) ) ;
#9797 = CARTESIAN_POINT ( 'NONE',  ( 0.000000000000000000, -84.33453774737664332, 11.08490790852103380 ) ) ;
#9798 = PRESENTATION_STYLE_ASSIGNMENT (( #14793 ) ) ;
#9799 = AXIS2_PLACEMENT_3D ( 'NONE', #17258, #2119, #12055 ) ;
#9800 = AXIS2_PLACEMENT_3D ( 'NONE', #4241, #9299, #14280 ) ;
#9801 = VECTOR ( 'NONE', #146, 1000.000000000000000 ) ;
#9802 = DIRECTION ( 'NONE',  ( 0.000000000000000000, -0.06975647374411146628, -0.9975640502598251969 ) ) ;
#9803 = CYLINDRICAL_SURFACE ( 'NONE', #2911, 92.50100000000000477 ) ;
#9804 = AXIS2_PLACEMENT_3D ( 'NONE', #20621, #18753, #306 ) ;
#9805 = AXIS2_PLACEMENT_3D ( 'NONE', #5551, #18601, #2016 ) ;
#9806 = FACE_OUTER_BOUND ( 'NONE', #2188, .T. ) ;
#9807 = DIRECTION ( 'NONE',  ( -1.000000000000000000, 0.000000000000000000, 0.000000000000000000 ) ) ;
#9808 = FACE_OUTER_BOUND ( 'NONE', #15793, .T. ) ;
#9809 = DIRECTION ( 'NONE',  ( 1.000000000000000000, 0.000000000000000000, 0.000000000000000000 ) ) ;
#9810 =( REPRESENTATION_RELATIONSHIP ('NONE','NONE', #2177, #14169 ) REPRESENTATION_RELATIONSHIP_WITH_TRANSFORMATION ( #3449 )SHAPE_REPRESENTATION_RELATIONSHIP( ) );
#9811 = ORIENTED_EDGE ( 'NONE', *, *, #555, .F. ) ;
#9812 = EDGE_CURVE ( 'NONE', #12235, #21050, #2968, .T. ) ;
#9813 = ORIENTED_EDGE ( 'NONE', *, *, #3559, .T. ) ;
#9814 = VERTEX_POINT ( 'NONE', #17975 ) ;
#9815 = VECTOR ( 'NONE', #15808, 1000.000000000000000 ) ;
#9816 = ORIENTED_EDGE ( 'NONE', *, *, #19063, .F. ) ;
#9817 = CIRCLE ( 'NONE', #16883, 44.99999999999999289 ) ;
#9818 = CIRCLE ( 'NONE', #315, 44.99999999999998579 ) ;
#9819 = CIRCLE ( 'NONE', #19704, 12.00000000000000000 ) ;
#9820 = AXIS2_PLACEMENT_3D ( 'NONE', #8298, #1115, #16355 ) ;
#9821 = ADVANCED_FACE ( 'NONE', ( #19620, #9652 ), #4486, .T. ) ;
#9822 = VERTEX_POINT ( 'NONE', #20061 ) ;
#9823 = DIRECTION ( 'NONE',  ( -1.000000000000000000, -0.000000000000000000, -0.000000000000000000 ) ) ;
#9824 = ORIENTED_EDGE ( 'NONE', *, *, #6756, .F. ) ;
#9825 = CARTESIAN_POINT ( 'NONE',  ( 10.00000000000000000, -67.05625154133410604, -63.71729851637880415 ) ) ;
#9826 = DIRECTION ( 'NONE',  ( -1.000000000000000000, 0.000000000000000000, -0.000000000000000000 ) ) ;
#9827 = DIRECTION ( 'NONE',  ( -1.000000000000000000, 0.000000000000000000, 0.000000000000000000 ) ) ;
#9828 = DIRECTION ( 'NONE',  ( 1.000000000000000000, 0.000000000000000000, 0.000000000000000000 ) ) ;
#9829 = PRESENTATION_STYLE_ASSIGNMENT (( #1224 ) ) ;
#9830 = AXIS2_PLACEMENT_3D ( 'NONE', #4375, #16199, #9550 ) ;
#9831 = CARTESIAN_POINT ( 'NONE',  ( -90.00000000000000000, 0.000000000000000000, -100.0000000000000284 ) ) ;
#9832 = FACE_OUTER_BOUND ( 'NONE', #4833, .T. ) ;
#9833 = CIRCLE ( 'NONE', #15838, 88.00000000000000000 ) ;
#9834 = CIRCLE ( 'NONE', #19370, 3.000000000000000000 ) ;
#9835 = CIRCLE ( 'NONE', #332, 45.00000000000000000 ) ;
#9836 = VERTEX_POINT ( 'NONE', #16195 ) ;
#9837 = PRODUCT_DEFINITION_SHAPE ( 'NONE', 'NONE',  #9257 ) ;
#9838 = CYLINDRICAL_SURFACE ( 'NONE', #3743, 88.00000000000000000 ) ;
#9839 = EDGE_CURVE ( 'NONE', #5806, #18737, #8616, .T. ) ;
#9840 = EDGE_CURVE ( 'NONE', #19664, #6016, #5450, .T. ) ;
#9841 = ORIENTED_EDGE ( 'NONE', *, *, #14843, .T. ) ;
#9842 = ORIENTED_EDGE ( 'NONE', *, *, #16472, .F. ) ;
#9843 = DIRECTION ( 'NONE',  ( 0.000000000000000000, 0.000000000000000000, 1.000000000000000000 ) ) ;
#9844 = ORIENTED_EDGE ( 'NONE', *, *, #16128, .F. ) ;
#9845 = CARTESIAN_POINT ( 'NONE',  ( 0.000000000000000000, 0.000000000000000000, 0.000000000000000000 ) ) ;
#9846 = ORIENTED_EDGE ( 'NONE', *, *, #16532, .F. ) ;
#9847 = ORIENTED_EDGE ( 'NONE', *, *, #2741, .F. ) ;
#9848 = CONTEXT_DEPENDENT_SHAPE_REPRESENTATION ( #6447, #8618 ) ;
#9849 = VECTOR ( 'NONE', #8050, 1000.000000000000000 ) ;
#9850 = CYLINDRICAL_SURFACE ( 'NONE', #12263, 44.99999999999999289 ) ;
#9851 = VERTEX_POINT ( 'NONE', #9438 ) ;
#9852 = AXIS2_PLACEMENT_3D ( 'NONE', #1945, #3822, #397 ) ;
#9853 = DIRECTION ( 'NONE',  ( 0.000000000000000000, 0.5877852522924689183, 0.8090169943749504489 ) ) ;
#9854 = AXIS2_PLACEMENT_3D ( 'NONE', #8794, #14187, #20934 ) ;
#9855 = AXIS2_PLACEMENT_3D ( 'NONE', #2278, #4270, #7588 ) ;
#9856 = DIRECTION ( 'NONE',  ( 0.000000000000000000, 0.000000000000000000, 1.000000000000000000 ) ) ;
#9857 = ADVANCED_FACE ( 'NONE', ( #19728 ), #11553, .F. ) ;
#9858 = CYLINDRICAL_SURFACE ( 'NONE', #15344, 11.99999999999999822 ) ;
#9859 = DIRECTION ( 'NONE',  ( -1.000000000000000000, 0.000000000000000000, 0.000000000000000000 ) ) ;
#9860 = CARTESIAN_POINT ( 'NONE',  ( 10.00000000000000000, 11.59241532900744787, -87.23311244498727035 ) ) ;
#9861 = CARTESIAN_POINT ( 'NONE',  ( 10.00000000000000000, 0.000000000000000000, 0.000000000000000000 ) ) ;
#9862 = EDGE_CURVE ( 'NONE', #2871, #19585, #8277, .T. ) ;
#9863 = CARTESIAN_POINT ( 'NONE',  ( 10.00000000000000000, 25.56104204395304080, 81.12843256239672485 ) ) ;
#9864 = DIRECTION ( 'NONE',  ( -1.000000000000000000, 0.000000000000000000, 0.000000000000000000 ) ) ;
#9865 = EDGE_LOOP ( 'NONE', ( #19901, #3715 ) ) ;
#9866 = EDGE_CURVE ( 'NONE', #19686, #7874, #8967, .T. ) ;
#9867 = EDGE_CURVE ( 'NONE', #21189, #1350, #11323, .T. ) ;
#9868 = ADVANCED_FACE ( 'NONE', ( #17860 ), #7907, .T. ) ;
#9869 = CIRCLE ( 'NONE', #16234, 45.00000000000000000 ) ;
#9870 = VECTOR ( 'NONE', #10323, 1000.000000000000000 ) ;
#9871 = CYLINDRICAL_SURFACE ( 'NONE', #16504, 92.50100000000000477 ) ;
#9872 = ADVANCED_FACE ( 'NONE', ( #16408 ), #19829, .F. ) ;
#9873 = DIRECTION ( 'NONE',  ( -1.000000000000000000, -0.000000000000000000, -0.000000000000000000 ) ) ;
#9874 = VERTEX_POINT ( 'NONE', #14862 ) ;
#9875 = DIRECTION ( 'NONE',  ( -0.000000000000000000, -0.000000000000000000, -1.000000000000000000 ) ) ;
#9876 = VERTEX_POINT ( 'NONE', #18072 ) ;
#9877 = VERTEX_POINT ( 'NONE', #2927 ) ;
#9878 = CYLINDRICAL_SURFACE ( 'NONE', #1163, 44.99999999999999289 ) ;
#9879 = EDGE_LOOP ( 'NONE', ( #21186, #9759, #4719, #20825 ) ) ;
#9880 = ORIENTED_EDGE ( 'NONE', *, *, #10402, .F. ) ;
#9881 = DIRECTION ( 'NONE',  ( 1.000000000000000000, 0.000000000000000000, 0.000000000000000000 ) ) ;
#9882 = DIRECTION ( 'NONE',  ( 0.000000000000000000, 0.9510565162951544194, -0.3090169943749448977 ) ) ;
#9883 = ORIENTED_EDGE ( 'NONE', *, *, #6273, .F. ) ;
#9884 = EDGE_CURVE ( 'NONE', #8891, #3599, #8232, .T. ) ;
#9885 = CARTESIAN_POINT ( 'NONE',  ( -140.0000507999999968, 0.000000000000000000, 0.000000000000000000 ) ) ;
#9886 = CARTESIAN_POINT ( 'NONE',  ( 10.00000000000000000, 16.79755869217650144, 90.96305306542258506 ) ) ;
#9887 = FACE_OUTER_BOUND ( 'NONE', #7089, .T. ) ;
#9888 = AXIS2_PLACEMENT_3D ( 'NONE', #7864, #14600, #19361 ) ;
#9889 = EDGE_CURVE ( 'NONE', #19281, #15418, #20261, .T. ) ;
#9890 = DIRECTION ( 'NONE',  ( 1.000000000000000000, 0.000000000000000000, 0.000000000000000000 ) ) ;
#9891 = DIRECTION ( 'NONE',  ( 0.000000000000000000, 0.000000000000000000, 1.000000000000000000 ) ) ;
#9892 = DIRECTION ( 'NONE',  ( -1.000000000000000000, -0.000000000000000000, -0.000000000000000000 ) ) ;
#9893 = UNCERTAINTY_MEASURE_WITH_UNIT (LENGTH_MEASURE( 1.000000000000000082E-05 ), #8797, 'distance_accuracy_value', 'NONE');
#9894 = ORIENTED_EDGE ( 'NONE', *, *, #12333, .T. ) ;
#9895 = EDGE_CURVE ( 'NONE', #2536, #2434, #21598, .T. ) ;
#9896 = CARTESIAN_POINT ( 'NONE',  ( 1.399999999999998579, 0.000000000000000000, 0.000000000000000000 ) ) ;
#9897 = DIRECTION ( 'NONE',  ( -1.000000000000000000, 0.000000000000000000, -0.000000000000000000 ) ) ;
#9898 = EDGE_LOOP ( 'NONE', ( #13765, #15887, #11297, #14551 ) ) ;
#9899 = CARTESIAN_POINT ( 'NONE',  ( 10.00000000000000000, 91.49386717542239467, -13.61276130276895557 ) ) ;
#9900 = ORIENTED_EDGE ( 'NONE', *, *, #13116, .T. ) ;
#9901 = ADVANCED_FACE ( 'NONE', ( #3045 ), #16524, .F. ) ;
#9902 = CARTESIAN_POINT ( 'NONE',  ( 10.00000000000000000, 12.90282758293013643, -25.06465718894764194 ) ) ;
#9903 = CIRCLE ( 'NONE', #4611, 45.00000000000000000 ) ;
#9904 = CARTESIAN_POINT ( 'NONE',  ( 10.00000000000000000, -85.05652083079338865, -0.7600687895868707411 ) ) ;
#9905 = ORIENTED_EDGE ( 'NONE', *, *, #5698, .T. ) ;
#9906 = CARTESIAN_POINT ( 'NONE',  ( 10.00000000000000000, 0.000000000000000000, 0.000000000000000000 ) ) ;
#9907 = ORIENTED_EDGE ( 'NONE', *, *, #18891, .F. ) ;
#9908 = ORIENTED_EDGE ( 'NONE', *, *, #19434, .F. ) ;
#9909 = LINE ( 'NONE', #16651, #9374 ) ;
#9910 = ORIENTED_EDGE ( 'NONE', *, *, #8959, .F. ) ;
#9911 = CARTESIAN_POINT ( 'NONE',  ( 0.000000000000000000, 61.71252885873465033, -58.53847642588533517 ) ) ;
#9912 = CYLINDRICAL_SURFACE ( 'NONE', #10051, 12.00000000000000000 ) ;
#9913 = CARTESIAN_POINT ( 'NONE',  ( -2.000000000000000000, 70.00000000000000000, 9.999999999999998224 ) ) ;
#9914 = DIRECTION ( 'NONE',  ( -1.000000000000000000, -0.000000000000000000, -0.000000000000000000 ) ) ;
#9915 = EDGE_CURVE ( 'NONE', #11955, #3827, #5122, .T. ) ;
#9916 = CARTESIAN_POINT ( 'NONE',  ( 10.00000000000000000, 7.409634587003466777, -27.19958299168149907 ) ) ;
#9917 = DIRECTION ( 'NONE',  ( -1.000000000000000000, 0.000000000000000000, -0.000000000000000000 ) ) ;
#9918 = CARTESIAN_POINT ( 'NONE',  ( 9.999999999999980460, 0.000000000000000000, 0.000000000000000000 ) ) ;
#9919 = PRESENTATION_LAYER_ASSIGNMENT (  '', '', ( #1101 ) ) ;
#9920 = ADVANCED_FACE ( 'NONE', ( #13308 ), #13851, .F. ) ;
#9921 = CARTESIAN_POINT ( 'NONE',  ( 0.000000000000000000, 0.000000000000000000, 0.000000000000000000 ) ) ;
#9922 = DIRECTION ( 'NONE',  ( 0.000000000000000000, 0.000000000000000000, 1.000000000000000000 ) ) ;
#9923 = CARTESIAN_POINT ( 'NONE',  ( 0.000000000000000000, 51.76708072107885528, 67.49339815138510801 ) ) ;
#9924 = VERTEX_POINT ( 'NONE', #13753 ) ;
#9925 =( NAMED_UNIT ( * ) PLANE_ANGLE_UNIT ( ) SI_UNIT ( $, .RADIAN. ) );
#9926 = ORIENTED_EDGE ( 'NONE', *, *, #3168, .T. ) ;
#9927 = VERTEX_POINT ( 'NONE', #6709 ) ;
#9928 = ORIENTED_EDGE ( 'NONE', *, *, #3394, .F. ) ;
#9929 = VECTOR ( 'NONE', #493, 1000.000000000000000 ) ;
#9930 = AXIS2_PLACEMENT_3D ( 'NONE', #4232, #6013, #16157 ) ;
#9931 = VERTEX_POINT ( 'NONE', #164 ) ;
#9932 = CARTESIAN_POINT ( 'NONE',  ( 10.00000000000000000, -39.87723064937176076, 83.46401306393555330 ) ) ;
#9933 = ORIENTED_EDGE ( 'NONE', *, *, #21745, .F. ) ;
#9934 = DIRECTION ( 'NONE',  ( -1.000000000000000000, -0.000000000000000000, -0.000000000000000000 ) ) ;
#9936 = ADVANCED_FACE ( 'NONE', ( #3480 ), #1602, .F. ) ;
#9935 = DIRECTION ( 'NONE',  ( -1.000000000000000000, -0.000000000000000000, -0.000000000000000000 ) ) ;
#9937 = CARTESIAN_POINT ( 'NONE',  ( 10.00000000000000000, -67.05625154133495869, 63.71729851637790176 ) ) ;
#9938 = DIRECTION ( 'NONE',  ( -1.000000000000000000, -0.000000000000000000, -0.000000000000000000 ) ) ;
#9939 = FACE_OUTER_BOUND ( 'NONE', #7464, .T. ) ;
#9940 = DIRECTION ( 'NONE',  ( 0.000000000000000000, -9.251858538542971828E-16, -1.000000000000000000 ) ) ;
#9941 = ORIENTED_EDGE ( 'NONE', *, *, #15632, .T. ) ;
#9942 = ORIENTED_EDGE ( 'NONE', *, *, #11752, .T. ) ;
#9943 = CARTESIAN_POINT ( 'NONE',  ( 0.000000000000000000, -17.83210509884655792, 21.83428559348755371 ) ) ;
#9944 = ORIENTED_EDGE ( 'NONE', *, *, #3499, .F. ) ;
#9945 = EDGE_LOOP ( 'NONE', ( #9288, #4985, #18634, #15936 ) ) ;
#9946 = CARTESIAN_POINT ( 'NONE',  ( -2.000000000000000000, 67.00000000000000000, 9.999999999999998224 ) ) ;
#9947 = CIRCLE ( 'NONE', #19135, 88.00000000000000000 ) ;
#9948 = EDGE_LOOP ( 'NONE', ( #9894, #18747, #5397, #4440 ) ) ;
#9949 = DIRECTION ( 'NONE',  ( 0.000000000000000000, -0.7431448254773861395, -0.6691306063588672304 ) ) ;
#9950 = VERTEX_POINT ( 'NONE', #15072 ) ;
#9951 = ORIENTED_EDGE ( 'NONE', *, *, #9577, .F. ) ;
#9952 = CONTEXT_DEPENDENT_SHAPE_REPRESENTATION ( #13622, #6865 ) ;
#9953 = CARTESIAN_POINT ( 'NONE',  ( 10.00000000000000000, -27.00677879428973682, -80.65868421664460186 ) ) ;
#9954 = VERTEX_POINT ( 'NONE', #8344 ) ;
#9955 = FACE_OUTER_BOUND ( 'NONE', #11839, .T. ) ;
#9956 = CARTESIAN_POINT ( 'NONE',  ( 10.00000000000000000, 91.70173545986517638, 12.13370160540072362 ) ) ;
#9957 = AXIS2_PLACEMENT_3D ( 'NONE', #6883, #10187, #132 ) ;
#9958 = LINE ( 'NONE', #18383, #880 ) ;
#9959 = CARTESIAN_POINT ( 'NONE',  ( 10.00000000000000000, 0.000000000000000000, 0.000000000000000000 ) ) ;
#9960 = EDGE_CURVE ( 'NONE', #6192, #783, #18510, .T. ) ;
#9961 = CARTESIAN_POINT ( 'NONE',  ( 0.000000000000000000, -23.10190250628894404, 89.56973317806591695 ) ) ;
#9962 = CYLINDRICAL_SURFACE ( 'NONE', #6158, 12.00000000000000000 ) ;
#9963 = CARTESIAN_POINT ( 'NONE',  ( 0.000000000000000000, 0.000000000000000000, 0.000000000000000000 ) ) ;
#9964 = DIRECTION ( 'NONE',  ( 1.000000000000000000, 0.000000000000000000, 0.000000000000000000 ) ) ;
#9965 = ORIENTED_EDGE ( 'NONE', *, *, #11342, .T. ) ;
#9966 = ADVANCED_FACE ( 'NONE', ( #2036 ), #3585, .F. ) ;
#9967 = VECTOR ( 'NONE', #1965, 1000.000000000000000 ) ;
#9968 = DIRECTION ( 'NONE',  ( 0.000000000000000000, 0.000000000000000000, 1.000000000000000000 ) ) ;
#9969 = EDGE_CURVE ( 'NONE', #667, #11653, #6914, .T. ) ;
#9970 = CARTESIAN_POINT ( 'NONE',  ( 5.000000000000000888, -7.240962358591358061, -31.16999300804322104 ) ) ;
#9971 = VECTOR ( 'NONE', #1442, 1000.000000000000000 ) ;
#9972 = ORIENTED_EDGE ( 'NONE', *, *, #11267, .T. ) ;
#9973 = DIRECTION ( 'NONE',  ( 1.000000000000000000, 0.000000000000000000, -0.000000000000000000 ) ) ;
#9974 = ORIENTED_EDGE ( 'NONE', *, *, #1769, .T. ) ;
#9975 =( NAMED_UNIT ( * ) SI_UNIT ( $, .STERADIAN. ) SOLID_ANGLE_UNIT ( ) );
#9976 = ORIENTED_EDGE ( 'NONE', *, *, #29, .T. ) ;
#9977 = DIRECTION ( 'NONE',  ( 1.000000000000000000, 0.000000000000000000, -0.000000000000000000 ) ) ;
#9978 = EDGE_LOOP ( 'NONE', ( #6707, #18117, #2347, #16336 ) ) ;
#9979 = ORIENTED_EDGE ( 'NONE', *, *, #7566, .F. ) ;
#9980 = DIRECTION ( 'NONE',  ( -1.000000000000000000, 0.000000000000000000, 0.000000000000000000 ) ) ;
#9981 = DIRECTION ( 'NONE',  ( 0.000000000000000000, 0.000000000000000000, 1.000000000000000000 ) ) ;
#9982 = AXIS2_PLACEMENT_3D ( 'NONE', #701, #15725, #17501 ) ;
#9983 = ORIENTED_EDGE ( 'NONE', *, *, #5692, .T. ) ;
#9984 = EDGE_CURVE ( 'NONE', #17955, #14440, #14625, .T. ) ;
#9985 = FACE_OUTER_BOUND ( 'NONE', #10358, .T. ) ;
#9986 = CARTESIAN_POINT ( 'NONE',  ( 0.000000000000000000, 0.000000000000000000, -3.000000000000000000 ) ) ;
#9987 = EDGE_CURVE ( 'NONE', #5218, #11931, #17108, .T. ) ;
#9988 = CARTESIAN_POINT ( 'NONE',  ( 10.00000000000000000, 7.240962358591984227, -31.16999300804307182 ) ) ;
#9989 = ADVANCED_FACE ( 'NONE', ( #12083 ), #8459, .F. ) ;
#9990 = DIRECTION ( 'NONE',  ( -1.000000000000000000, 0.000000000000000000, 0.000000000000000000 ) ) ;
#9991 = CARTESIAN_POINT ( 'NONE',  ( 10.00000000000000000, 0.000000000000000000, 0.000000000000000000 ) ) ;
#9992 = DIRECTION ( 'NONE',  ( 0.000000000000000000, 0.000000000000000000, 1.000000000000000000 ) ) ;
#9993 = EDGE_CURVE ( 'NONE', #5530, #2619, #8774, .T. ) ;
#9994 = AXIS2_PLACEMENT_3D ( 'NONE', #15212, #13226, #18221 ) ;
#9995 = ORIENTED_EDGE ( 'NONE', *, *, #276, .T. ) ;
#9996 = DIRECTION ( 'NONE',  ( -1.000000000000000000, 0.000000000000000000, 0.000000000000000000 ) ) ;
#9997 = CIRCLE ( 'NONE', #9623, 7.500000000000020428 ) ;
#9998 = CARTESIAN_POINT ( 'NONE',  ( 0.000000000000000000, 27.00677879429135331, -80.65868421664406185 ) ) ;
#9999 = EDGE_LOOP ( 'NONE', ( #17024, #2621, #14830, #14444 ) ) ;
#10000 = AXIS2_PLACEMENT_3D ( 'NONE', #20943, #4153, #9219 ) ;
#10001 = DIRECTION ( 'NONE',  ( 0.000000000000000000, 0.000000000000000000, 1.000000000000000000 ) ) ;
#10002 = EDGE_CURVE ( 'NONE', #6908, #5130, #20167, .T. ) ;
#10003 = ORIENTED_EDGE ( 'NONE', *, *, #31, .F. ) ;
#10004 = CARTESIAN_POINT ( 'NONE',  ( 0.000000000000000000, 15.51843147776349063, 83.63233659819657362 ) ) ;
#10005 = DIRECTION ( 'NONE',  ( -1.000000000000000000, -0.000000000000000000, -0.000000000000000000 ) ) ;
#10006 = ORIENTED_EDGE ( 'NONE', *, *, #21344, .F. ) ;
#10007 = DIRECTION ( 'NONE',  ( 0.000000000000000000, 0.000000000000000000, -1.000000000000000000 ) ) ;
#10008 = EDGE_CURVE ( 'NONE', #8011, #7101, #13635, .T. ) ;
#10009 = AXIS2_PLACEMENT_3D ( 'NONE', #14107, #9441, #16198 ) ;
#10010 = ORIENTED_EDGE ( 'NONE', *, *, #16868, .T. ) ;
#10011 = EDGE_LOOP ( 'NONE', ( #303, #6636, #9217, #7958 ) ) ;
#10012 = PLANE ( 'NONE',  #18485 ) ;
#10013 = ORIENTED_EDGE ( 'NONE', *, *, #10086, .T. ) ;
#10014 = CARTESIAN_POINT ( 'NONE',  ( 10.00000000000000000, 26.27606311335965827, -10.21217444509384364 ) ) ;
#10015 = AXIS2_PLACEMENT_3D ( 'NONE', #8879, #20821, #710 ) ;
#10016 = CYLINDRICAL_SURFACE ( 'NONE', #18897, 44.99999999999999289 ) ;
#10017 = CARTESIAN_POINT ( 'NONE',  ( 0.000000000000000000, 29.29369617358583255, -87.74003855418371245 ) ) ;
#10018 = DIRECTION ( 'NONE',  ( -1.000000000000000000, -0.000000000000000000, -0.000000000000000000 ) ) ;
#10019 =( NAMED_UNIT ( * ) PLANE_ANGLE_UNIT ( ) SI_UNIT ( $, .RADIAN. ) );
#10020 = EDGE_CURVE ( 'NONE', #13874, #7135, #10427, .T. ) ;
#10021 = FACE_OUTER_BOUND ( 'NONE', #6436, .T. ) ;
#10022 = DIRECTION ( 'NONE',  ( 0.000000000000000000, -0.4694715627858797591, -0.8829475928589327616 ) ) ;
#10023 = CYLINDRICAL_SURFACE ( 'NONE', #17632, 44.99999999999999289 ) ;
#10024 = VECTOR ( 'NONE', #5029, 1000.000000000000000 ) ;
#10025 = DIRECTION ( 'NONE',  ( 0.000000000000000000, 0.000000000000000000, 1.000000000000000000 ) ) ;
#10026 = DIRECTION ( 'NONE',  ( 1.000000000000000000, 0.000000000000000000, 0.000000000000000000 ) ) ;
#10027 = ADVANCED_FACE ( 'NONE', ( #9985 ), #16963, .T. ) ;
#10028 = CIRCLE ( 'NONE', #16017, 45.00000000000000000 ) ;
#10029 = VERTEX_POINT ( 'NONE', #11763 ) ;
#10030 = DIRECTION ( 'NONE',  ( -1.000000000000000000, 0.000000000000000000, -0.000000000000000000 ) ) ;
#10031 = ORIENTED_EDGE ( 'NONE', *, *, #17211, .T. ) ;
#10032 = CARTESIAN_POINT ( 'NONE',  ( 10.00000000000000000, 3.728035544477412255, -84.97818067823766341 ) ) ;
#10033 = ADVANCED_FACE ( 'NONE', ( #18836 ), #8986, .T. ) ;
#10034 = AXIS2_PLACEMENT_3D ( 'NONE', #20385, #18729, #3583 ) ;
#10035 = ORIENTED_EDGE ( 'NONE', *, *, #4083, .T. ) ;
#10036 = VERTEX_POINT ( 'NONE', #10315 ) ;
#10037 = EDGE_CURVE ( 'NONE', #21406, #19754, #6538, .T. ) ;
#10038 = ADVANCED_FACE ( 'NONE', ( #4929 ), #4240, .F. ) ;
#10039 = VERTEX_POINT ( 'NONE', #5900 ) ;
#10040 = FACE_OUTER_BOUND ( 'NONE', #695, .T. ) ;
#10041 = CIRCLE ( 'NONE', #521, 88.00000000000000000 ) ;
#10042 = ORIENTED_EDGE ( 'NONE', *, *, #19630, .F. ) ;
#10043 = DIRECTION ( 'NONE',  ( 0.000000000000000000, 3.546545773108138773E-15, -1.000000000000000000 ) ) ;
#10044 = AXIS2_PLACEMENT_3D ( 'NONE', #12347, #2178, #15216 ) ;
#10045 = CARTESIAN_POINT ( 'NONE',  ( 10.00000000000000000, 0.000000000000000000, 0.000000000000000000 ) ) ;
#10046 = AXIS2_PLACEMENT_3D ( 'NONE', #4281, #11016, #17769 ) ;
#10048 = CIRCLE ( 'NONE', #528, 44.99999999999998579 ) ;
#10047 = AXIS2_PLACEMENT_3D ( 'NONE', #20596, #10971, #21032 ) ;
#10049 = CARTESIAN_POINT ( 'NONE',  ( 0.000000000000000000, 16.79755869217650144, 90.96305306542258506 ) ) ;
#10050 = DIRECTION ( 'NONE',  ( -1.000000000000000000, 0.000000000000000000, 0.000000000000000000 ) ) ;
#10051 = AXIS2_PLACEMENT_3D ( 'NONE', #3183, #16765, #7934 ) ;
#10052 = CARTESIAN_POINT ( 'NONE',  ( 0.000000000000000000, -18.94217447942500598, -85.93715160505971085 ) ) ;
#10053 = CARTESIAN_POINT ( 'NONE',  ( 0.000000000000000000, 0.000000000000000000, 0.000000000000000000 ) ) ;
#10054 = ORIENTED_EDGE ( 'NONE', *, *, #15783, .T. ) ;
#10055 = FACE_OUTER_BOUND ( 'NONE', #21857, .T. ) ;
#10056 = AXIS2_PLACEMENT_3D ( 'NONE', #9528, #20923, #16606 ) ;
#10057 = TOROIDAL_SURFACE ( 'NONE', #10405, 118.9000000000000199, 1.100000000000009859 ) ;
#10058 = ORIENTED_EDGE ( 'NONE', *, *, #17728, .F. ) ;
#10059 = CIRCLE ( 'NONE', #545, 92.50100000000001899 ) ;
#10060 = ORIENTED_EDGE ( 'NONE', *, *, #17047, .F. ) ;
#10061 = CIRCLE ( 'NONE', #7944, 88.00000000000000000 ) ;
#10062 = DIRECTION ( 'NONE',  ( -1.000000000000000000, 0.000000000000000000, -0.000000000000000000 ) ) ;
#10063 = ORIENTED_EDGE ( 'NONE', *, *, #16907, .T. ) ;
#10064 = DIRECTION ( 'NONE',  ( 0.000000000000000000, 0.000000000000000000, 1.000000000000000000 ) ) ;
#10065 = ORIENTED_EDGE ( 'NONE', *, *, #991, .T. ) ;
#10066 = ORIENTED_EDGE ( 'NONE', *, *, #21759, .F. ) ;
#10067 = CONTEXT_DEPENDENT_SHAPE_REPRESENTATION ( #2758, #18498 ) ;
#10068 = CARTESIAN_POINT ( 'NONE',  ( 10.00000000000000000, 0.000000000000000000, 0.000000000000000000 ) ) ;
#10069 = ORIENTED_EDGE ( 'NONE', *, *, #4777, .T. ) ;
#10070 = CLOSED_SHELL ( 'NONE', ( #2713, #14730, #11357, #21751, #18490, #21316, #3075, #11678, #18818, #20531, #17338, #11384 ) ) ;
#10071 = CYLINDRICAL_SURFACE ( 'NONE', #13388, 27.49900000000000233 ) ;
#10072 = CARTESIAN_POINT ( 'NONE',  ( 10.00000000000000000, -15.51843147776295950, -83.63233659819665888 ) ) ;
#10073 = DIRECTION ( 'NONE',  ( -1.000000000000000000, -0.000000000000000000, -0.000000000000000000 ) ) ;
#10074 = CIRCLE ( 'NONE', #3727, 88.00000000000000000 ) ;
#10075 = DIRECTION ( 'NONE',  ( 0.000000000000000000, -0.4067366430757887730, -0.9135454576426059736 ) ) ;
#10076 = CIRCLE ( 'NONE', #13613, 45.00000000000000711 ) ;
#10077 = AXIS2_PLACEMENT_3D ( 'NONE', #10640, #21252, #14399 ) ;
#10078 = DIRECTION ( 'NONE',  ( 0.000000000000000000, 0.000000000000000000, 1.000000000000000000 ) ) ;
#10079 = DIRECTION ( 'NONE',  ( -1.000000000000000000, 0.000000000000000000, -0.000000000000000000 ) ) ;
#10081 = CIRCLE ( 'NONE', #21031, 88.00000000000000000 ) ;
#10080 = LINE ( 'NONE', #3343, #20043 ) ;
#10082 = ORIENTED_EDGE ( 'NONE', *, *, #14082, .T. ) ;
#10083 = CARTESIAN_POINT ( 'NONE',  ( 0.000000000000000000, 0.000000000000000000, 0.000000000000000000 ) ) ;
#10084 = CYLINDRICAL_SURFACE ( 'NONE', #8822, 92.50100000000000477 ) ;
#10085 = ORIENTED_EDGE ( 'NONE', *, *, #17435, .F. ) ;
#10086 = EDGE_CURVE ( 'NONE', #12373, #2852, #12497, .T. ) ;
#10087 = CIRCLE ( 'NONE', #574, 92.50100000000001899 ) ;
#10088 = CARTESIAN_POINT ( 'NONE',  ( 10.00000000000000000, -85.22372865846305956, 21.92979875759597874 ) ) ;
#10089 = ORIENTED_EDGE ( 'NONE', *, *, #2034, .F. ) ;
#10090 = AXIS2_PLACEMENT_3D ( 'NONE', #3228, #1140, #14836 ) ;
#10091 =( LENGTH_UNIT ( ) NAMED_UNIT ( * ) SI_UNIT ( .MILLI., .METRE. ) );
#10092 = AXIS2_PLACEMENT_3D ( 'NONE', #3179, #6403, #16434 ) ;
#10093 = ORIENTED_EDGE ( 'NONE', *, *, #12403, .F. ) ;
#10094 = DIRECTION ( 'NONE',  ( -1.000000000000000000, -0.000000000000000000, -0.000000000000000000 ) ) ;
#10095 = ORIENTED_EDGE ( 'NONE', *, *, #8491, .F. ) ;
#10096 = ORIENTED_EDGE ( 'NONE', *, *, #13922, .T. ) ;
#10097 = DIRECTION ( 'NONE',  ( -3.552713678800500929E-15, 0.000000000000000000, 1.000000000000000000 ) ) ;
#10098 = CARTESIAN_POINT ( 'NONE',  ( 10.00000000000000000, -68.36541360927220978, 50.60987712331682076 ) ) ;
#10099 = EDGE_CURVE ( 'NONE', #3139, #10994, #1582, .T. ) ;
#10100 = ORIENTED_EDGE ( 'NONE', *, *, #17539, .T. ) ;
#10101 = DIRECTION ( 'NONE',  ( 0.000000000000000000, 0.000000000000000000, 1.000000000000000000 ) ) ;
#10102 = CARTESIAN_POINT ( 'NONE',  ( 10.00000000000000888, 0.000000000000000000, -118.9000000000000199 ) ) ;
#10103 = DIRECTION ( 'NONE',  ( -1.000000000000000000, 0.000000000000000000, 0.000000000000000000 ) ) ;
#10104 = CARTESIAN_POINT ( 'NONE',  ( 0.000000000000000000, -3.728035544476815399, 84.97818067823770605 ) ) ;
#10105 = DIRECTION ( 'NONE',  ( 0.000000000000000000, -0.7431448254773997952, 0.6691306063588520203 ) ) ;
#10106 = CARTESIAN_POINT ( 'NONE',  ( 5.000000000000000000, 65.83713140174729972, 58.39068529131218099 ) ) ;
#10107 = AXIS2_PLACEMENT_3D ( 'NONE', #14468, #6077, #763 ) ;
#10108 = VERTEX_POINT ( 'NONE', #9095 ) ;
#10109 = AXIS2_PLACEMENT_3D ( 'NONE', #2657, #12711, #12278 ) ;
#10110 = CYLINDRICAL_SURFACE ( 'NONE', #1925, 44.99999999999999289 ) ;
#10111 = LINE ( 'NONE', #19248, #19257 ) ;
#10112 = ORIENTED_EDGE ( 'NONE', *, *, #9722, .F. ) ;
#10113 = CYLINDRICAL_SURFACE ( 'NONE', #19658, 88.00000000000000000 ) ;
#10114 = ORIENTED_EDGE ( 'NONE', *, *, #18141, .F. ) ;
#10115 = EDGE_CURVE ( 'NONE', #19966, #17806, #10638, .T. ) ;
#10116 = EDGE_CURVE ( 'NONE', #17553, #16041, #11109, .T. ) ;
#10117 = EDGE_CURVE ( 'NONE', #14712, #9088, #10537, .T. ) ;
#10118 = CARTESIAN_POINT ( 'NONE',  ( 10.00000000000000000, -29.29369617358527833, 87.74003855418389719 ) ) ;
#10119 = ORIENTED_EDGE ( 'NONE', *, *, #8835, .F. ) ;
#10120 = CARTESIAN_POINT ( 'NONE',  ( -8.900000000000019895, 0.000000000000000000, -120.0000000000000284 ) ) ;
#10121 = AXIS2_PLACEMENT_3D ( 'NONE', #3542, #12145, #17131 ) ;
#10122 = EDGE_CURVE ( 'NONE', #12701, #4580, #7926, .T. ) ;
#10123 = ORIENTED_EDGE ( 'NONE', *, *, #19078, .T. ) ;
#10124 = EDGE_LOOP ( 'NONE', ( #15810, #10791, #13220, #4177 ) ) ;
#10125 = AXIS2_PLACEMENT_3D ( 'NONE', #21721, #8146, #3057 ) ;
#10126 = ORIENTED_EDGE ( 'NONE', *, *, #16876, .T. ) ;
#10127 = DIRECTION ( 'NONE',  ( 0.000000000000000000, 0.9271838545667857590, 0.3746065934159160671 ) ) ;
#10128 = AXIS2_PLACEMENT_3D ( 'NONE', #3864, #5963, #20981 ) ;
#10129 = EDGE_LOOP ( 'NONE', ( #6319, #3003, #17174, #15603 ) ) ;
#10130 = CARTESIAN_POINT ( 'NONE',  ( -1.500000000000000444, 6.245698675651501825E-16, 5.100000000000000533 ) ) ;
#10131 = CARTESIAN_POINT ( 'NONE',  ( 10.00000000000000000, -74.74361964203257003, 40.60271866773520344 ) ) ;
#10132 = CARTESIAN_POINT ( 'NONE',  ( 0.000000000000000000, 0.000000000000000000, 0.000000000000000000 ) ) ;
#10133 = CARTESIAN_POINT ( 'NONE',  ( 5.000000000000002665, -87.44637528609668209, 9.855528870798345054 ) ) ;
#10134 = DIRECTION ( 'NONE',  ( -1.000000000000000000, 0.000000000000000000, 0.000000000000000000 ) ) ;
#10135 = ADVANCED_FACE ( 'NONE', ( #14074 ), #2355, .F. ) ;
#10136 = DIRECTION ( 'NONE',  ( 0.000000000000000000, 0.000000000000000000, -1.000000000000000000 ) ) ;
#10137 = EDGE_CURVE ( 'NONE', #11343, #16375, #18171, .T. ) ;
#10138 = CYLINDRICAL_SURFACE ( 'NONE', #20461, 88.00000000000000000 ) ;
#10139 = CIRCLE ( 'NONE', #21432, 44.99999999999999289 ) ;
#10140 = CARTESIAN_POINT ( 'NONE',  ( 10.00000000000000000, 7.409634587003093742, 27.19958299168160565 ) ) ;
#10141 = CIRCLE ( 'NONE', #9076, 115.1000000000000227 ) ;
#10142 = AXIS2_PLACEMENT_3D ( 'NONE', #14895, #1426, #11256 ) ;
#10143 = CARTESIAN_POINT ( 'NONE',  ( 1.400000000000000133, 0.000000000000000000, -5.100000000000000533 ) ) ;
#10144 = ORIENTED_EDGE ( 'NONE', *, *, #12048, .T. ) ;
#10145 = DIRECTION ( 'NONE',  ( 0.000000000000000000, 0.000000000000000000, 1.000000000000000000 ) ) ;
#10146 = EDGE_CURVE ( 'NONE', #2267, #8367, #14279, .T. ) ;
#10147 = VERTEX_POINT ( 'NONE', #2245 ) ;
#10148 = FACE_OUTER_BOUND ( 'NONE', #21103, .T. ) ;
#10149 = VERTEX_POINT ( 'NONE', #19376 ) ;
#10150 = EDGE_CURVE ( 'NONE', #12524, #19400, #5570, .T. ) ;
#10151 = ORIENTED_EDGE ( 'NONE', *, *, #12209, .F. ) ;
#10152 = ORIENTED_EDGE ( 'NONE', *, *, #14582, .T. ) ;
#10153 = CARTESIAN_POINT ( 'NONE',  ( 10.00000000000000000, -36.60317927562628881, 76.78148674856751654 ) ) ;
#10154 = CIRCLE ( 'NONE', #6642, 27.49900000000000588 ) ;
#10155 = AXIS2_PLACEMENT_3D ( 'NONE', #11191, #707, #17509 ) ;
#10156 = VERTEX_POINT ( 'NONE', #2569 ) ;
#10157 = FACE_OUTER_BOUND ( 'NONE', #10651, .T. ) ;
#10158 = CIRCLE ( 'NONE', #7001, 45.00000000000000000 ) ;
#10159 = CIRCLE ( 'NONE', #7686, 44.99999999999999289 ) ;
#10160 = CARTESIAN_POINT ( 'NONE',  ( 1.500000000000000000, 15.00000000000000000, 4.769696007084728073 ) ) ;
#10161 = EDGE_CURVE ( 'NONE', #21676, #13846, #2637, .T. ) ;
#10162 = DIRECTION ( 'NONE',  ( 0.000000000000000000, -0.8987940462991711454, 0.4383711467890689661 ) ) ;
#10163 = FACE_OUTER_BOUND ( 'NONE', #16712, .T. ) ;
#10164 = CYLINDRICAL_SURFACE ( 'NONE', #6531, 44.99999999999999289 ) ;
#10165 = EDGE_CURVE ( 'NONE', #1066, #14735, #14170, .T. ) ;
#10166 = CARTESIAN_POINT ( 'NONE',  ( 10.00000000000000000, -84.12297548659712731, -12.59025161327086906 ) ) ;
#10167 = AXIS2_PLACEMENT_3D ( 'NONE', #19028, #10073, #463 ) ;
#10168 = DIRECTION ( 'NONE',  ( -1.000000000000000000, 0.000000000000000000, 0.000000000000000000 ) ) ;
#10169 = ADVANCED_FACE ( 'NONE', ( #18943 ), #20817, .F. ) ;
#10170 = ORIENTED_EDGE ( 'NONE', *, *, #6670, .F. ) ;
#10171 = EDGE_CURVE ( 'NONE', #7364, #8570, #20915, .T. ) ;
#10172 = DIRECTION ( 'NONE',  ( 0.000000000000000000, -0.3420201433256757073, 0.9396926207859057634 ) ) ;
#10173 = AXIS2_PLACEMENT_3D ( 'NONE', #12271, #17476, #18801 ) ;
#10174 = VECTOR ( 'NONE', #11921, 1000.000000000000000 ) ;
#10175 = ORIENTED_EDGE ( 'NONE', *, *, #209, .F. ) ;
#10176 = CIRCLE ( 'NONE', #7361, 88.00000000000000000 ) ;
#10177 = AXIS2_PLACEMENT_3D ( 'NONE', #21123, #5884, #2779 ) ;
#10178 = VERTEX_POINT ( 'NONE', #19264 ) ;
#10179 = DIRECTION ( 'NONE',  ( 0.000000000000000000, 0.000000000000000000, 1.000000000000000000 ) ) ;
#10180 = EDGE_CURVE ( 'NONE', #9022, #569, #1220, .T. ) ;
#10181 = ORIENTED_EDGE ( 'NONE', *, *, #7850, .F. ) ;
#10182 = CARTESIAN_POINT ( 'NONE',  ( 0.000000000000000000, -23.37352460145268651, -21.85585385440903750 ) ) ;
#10183 = ORIENTED_EDGE ( 'NONE', *, *, #10825, .T. ) ;
#10184 = EDGE_LOOP ( 'NONE', ( #17341, #7875, #15777, #12948 ) ) ;
#10185 = DIRECTION ( 'NONE',  ( -1.000000000000000000, -0.000000000000000000, -0.000000000000000000 ) ) ;
#10186 = ORIENTED_EDGE ( 'NONE', *, *, #11113, .F. ) ;
#10187 = DIRECTION ( 'NONE',  ( -1.000000000000000000, -0.000000000000000000, 0.000000000000000000 ) ) ;
#10188 = CIRCLE ( 'NONE', #10895, 32.00000000000000000 ) ;
#10189 = DIRECTION ( 'NONE',  ( -1.000000000000000000, 0.000000000000000000, 0.000000000000000000 ) ) ;
#10190 = FACE_OUTER_BOUND ( 'NONE', #4552, .T. ) ;
#10191 = CIRCLE ( 'NONE', #11616, 88.00000000000000000 ) ;
#10192 = DIRECTION ( 'NONE',  ( 1.000000000000000000, 0.000000000000000000, 0.000000000000000000 ) ) ;
#10193 =( GEOMETRIC_REPRESENTATION_CONTEXT ( 3 ) GLOBAL_UNCERTAINTY_ASSIGNED_CONTEXT ( ( #1289 ) ) GLOBAL_UNIT_ASSIGNED_CONTEXT ( ( #15116, #9925, #18558 ) ) REPRESENTATION_CONTEXT ( 'NONE', 'WORKASPACE' ) );
#10194 = CIRCLE ( 'NONE', #666, 11.99999999999999822 ) ;
#10195 = CYLINDRICAL_SURFACE ( 'NONE', #14241, 11.99999999999999645 ) ;
#10196 = CARTESIAN_POINT ( 'NONE',  ( 0.000000000000000000, 0.000000000000000000, 3.000000000000000000 ) ) ;
#10197 = CARTESIAN_POINT ( 'NONE',  ( -1.500000000000001332, 0.000000000000000000, 0.000000000000000000 ) ) ;
#10198 = ORIENTED_EDGE ( 'NONE', *, *, #21759, .T. ) ;
#10199 = EDGE_CURVE ( 'NONE', #8423, #9701, #801, .T. ) ;
#10200 = CYLINDRICAL_SURFACE ( 'NONE', #12266, 11.99999999999999645 ) ;
#10201 = DIRECTION ( 'NONE',  ( 1.000000000000000000, 0.000000000000000000, -0.000000000000000000 ) ) ;
#10202 = ORIENTED_EDGE ( 'NONE', *, *, #3608, .T. ) ;
#10203 = AXIS2_PLACEMENT_3D ( 'NONE', #2819, #11207, #4027 ) ;
#10204 = PRESENTATION_LAYER_ASSIGNMENT (  '', '', ( #2802 ) ) ;
#10205 = DIRECTION ( 'NONE',  ( 0.000000000000000000, 0.000000000000000000, 1.000000000000000000 ) ) ;
#10207 = CIRCLE ( 'NONE', #13395, 44.99999999999999289 ) ;
#10206 = PRODUCT_DEFINITION_SHAPE ( 'NONE', 'NONE',  #5646 ) ;
#10208 = VERTEX_POINT ( 'NONE', #7546 ) ;
#10209 = SURFACE_STYLE_USAGE ( .BOTH. , #1705 ) ;
#10210 = ORIENTED_EDGE ( 'NONE', *, *, #9339, .T. ) ;
#10211 = CYLINDRICAL_SURFACE ( 'NONE', #1176, 88.00000000000000000 ) ;
#10212 = ORIENTED_EDGE ( 'NONE', *, *, #5269, .T. ) ;
#10213 = EDGE_LOOP ( 'NONE', ( #20480, #14636, #7390, #4881 ) ) ;
#10214 = FACE_OUTER_BOUND ( 'NONE', #2402, .T. ) ;
#10215 = CARTESIAN_POINT ( 'NONE',  ( 0.000000000000000000, 0.000000000000000000, 0.000000000000000000 ) ) ;
#10216 = ORIENTED_EDGE ( 'NONE', *, *, #4791, .F. ) ;
#10217 = CARTESIAN_POINT ( 'NONE',  ( 10.00000000000000000, -62.44821182181136976, 68.23969402963483333 ) ) ;
#10218 = CARTESIAN_POINT ( 'NONE',  ( 10.00000000000000000, -52.25832601289046409, -70.80301803122840454 ) ) ;
#10219 = DIRECTION ( 'NONE',  ( -1.000000000000000000, -0.000000000000000000, -0.000000000000000000 ) ) ;
#10220 = LINE ( 'NONE', #8878, #10720 ) ;
#10221 = CARTESIAN_POINT ( 'NONE',  ( 5.000000000000000000, 87.58454185039441597, 8.540961822681984117 ) ) ;
#10222 = LINE ( 'NONE', #3372, #10262 ) ;
#10223 = ADVANCED_FACE ( 'NONE', ( #12307 ), #11301, .F. ) ;
#10224 = VECTOR ( 'NONE', #5235, 1000.000000000000000 ) ;
#10225 = ORIENTED_EDGE ( 'NONE', *, *, #20015, .F. ) ;
#10226 = AXIS2_PLACEMENT_3D ( 'NONE', #6389, #2936, #19954 ) ;
#10227 = LINE ( 'NONE', #176, #9870 ) ;
#10228 = DIRECTION ( 'NONE',  ( 0.000000000000000000, 0.000000000000000000, 1.000000000000000000 ) ) ;
#10229 = EDGE_LOOP ( 'NONE', ( #20990, #12939, #8502, #9207 ) ) ;
#10230 = DIRECTION ( 'NONE',  ( 1.000000000000000000, -0.000000000000000000, -0.000000000000000000 ) ) ;
#10231 = EDGE_LOOP ( 'NONE', ( #9842, #18852, #8688, #2003 ) ) ;
#10232 = DIRECTION ( 'NONE',  ( 0.000000000000000000, 0.000000000000000000, 1.000000000000000000 ) ) ;
#10233 = DIRECTION ( 'NONE',  ( 0.000000000000000000, 0.000000000000000000, 1.000000000000000000 ) ) ;
#10234 = ORIENTED_EDGE ( 'NONE', *, *, #12260, .T. ) ;
#10235 = DIRECTION ( 'NONE',  ( 0.000000000000000000, -0.9945218953682744001, 0.1045284632676437564 ) ) ;
#10236 = ORIENTED_EDGE ( 'NONE', *, *, #1870, .F. ) ;
#10237 = ORIENTED_EDGE ( 'NONE', *, *, #10837, .F. ) ;
#10238 = ORIENTED_EDGE ( 'NONE', *, *, #6665, .F. ) ;
#10239 = CIRCLE ( 'NONE', #20481, 105.0992000000000104 ) ;
#10240 = CARTESIAN_POINT ( 'NONE',  ( 1.399999999999999245, 0.000000000000000000, 0.000000000000000000 ) ) ;
#10241 = ORIENTED_EDGE ( 'NONE', *, *, #2421, .T. ) ;
#10242 = DIRECTION ( 'NONE',  ( -1.000000000000000000, -0.000000000000000000, 0.000000000000000000 ) ) ;
#10243 = DIRECTION ( 'NONE',  ( -1.000000000000000000, -0.000000000000000000, 0.000000000000000000 ) ) ;
#10244 = CARTESIAN_POINT ( 'NONE',  ( 10.00000000000000000, 40.72878876293147954, 78.00747250042462611 ) ) ;
#10245 = DIRECTION ( 'NONE',  ( 0.000000000000000000, 0.000000000000000000, 1.000000000000000000 ) ) ;
#10246 = DIRECTION ( 'NONE',  ( 1.000000000000000000, -0.000000000000000000, -0.000000000000000000 ) ) ;
#10247 = ADVANCED_FACE ( 'NONE', ( #11526 ), #1250, .F. ) ;
#10248 = DIRECTION ( 'NONE',  ( 1.000000000000000000, -0.000000000000000000, -0.000000000000000000 ) ) ;
#10249 = CARTESIAN_POINT ( 'NONE',  ( 10.00000000000000000, 0.000000000000000000, 0.000000000000000000 ) ) ;
#10250 = CARTESIAN_POINT ( 'NONE',  ( 10.00000000000000000, 0.000000000000000000, 0.000000000000000000 ) ) ;
#10251 = FACE_OUTER_BOUND ( 'NONE', #8734, .T. ) ;
#10252 = CIRCLE ( 'NONE', #385, 92.50100000000000477 ) ;
#10253 = EDGE_CURVE ( 'NONE', #5782, #8283, #14397, .T. ) ;
#10254 = CARTESIAN_POINT ( 'NONE',  ( 10.00000000000000000, 24.17932380791719282, 20.96092317127012095 ) ) ;
#10255 = VERTEX_POINT ( 'NONE', #21575 ) ;
#10256 = LINE ( 'NONE', #3302, #10552 ) ;
#10257 = VERTEX_POINT ( 'NONE', #14509 ) ;
#10258 = CARTESIAN_POINT ( 'NONE',  ( 0.000000000000000000, 27.26034713664097353, 4.817140289263753594 ) ) ;
#10259 = VERTEX_POINT ( 'NONE', #4569 ) ;
#10260 = ADVANCED_FACE ( 'NONE', ( #21356 ), #1034, .F. ) ;
#10261 = VERTEX_POINT ( 'NONE', #19699 ) ;
#10262 = VECTOR ( 'NONE', #1288, 1000.000000000000000 ) ;
#10263 = EDGE_LOOP ( 'NONE', ( #6768, #20126 ) ) ;
#10264 = DIRECTION ( 'NONE',  ( 0.000000000000000000, -0.9271838545667832054, -0.3746065934159225619 ) ) ;
#10265 = ORIENTED_EDGE ( 'NONE', *, *, #11092, .T. ) ;
#10266 = CARTESIAN_POINT ( 'NONE',  ( 0.000000000000000000, 15.51843147776463638, -83.63233659819634624 ) ) ;
#10267 = CARTESIAN_POINT ( 'NONE',  ( 10.00000000000000000, 0.000000000000000000, 0.000000000000000000 ) ) ;
#10268 = EDGE_CURVE ( 'NONE', #15150, #4259, #21339, .T. ) ;
#10269 = CARTESIAN_POINT ( 'NONE',  ( 0.000000000000000000, 17.70753755129066320, -21.03896658273954046 ) ) ;
#10270 = EDGE_CURVE ( 'NONE', #8175, #18968, #3366, .T. ) ;
#10271 = CARTESIAN_POINT ( 'NONE',  ( 10.00000000000000000, 18.94217447942673971, -85.93715160505934136 ) ) ;
#10272 = DIRECTION ( 'NONE',  ( 0.000000000000000000, 0.000000000000000000, 1.000000000000000000 ) ) ;
#10273 = ADVANCED_FACE ( 'NONE', ( #6238, #19476 ), #4669, .T. ) ;
#10274 = CARTESIAN_POINT ( 'NONE',  ( 0.000000000000000000, 0.000000000000000000, 0.000000000000000000 ) ) ;
#10275 = LINE ( 'NONE', #1876, #7738 ) ;
#10276 = EDGE_CURVE ( 'NONE', #9836, #6661, #16057, .T. ) ;
#10277 = VERTEX_POINT ( 'NONE', #14614 ) ;
#10278 = CARTESIAN_POINT ( 'NONE',  ( 1.500000000000001332, 0.000000000000000000, -7.400000000000020783 ) ) ;
#10279 = AXIS2_PLACEMENT_3D ( 'NONE', #21141, #4330, #17820 ) ;
#10280 = ORIENTED_EDGE ( 'NONE', *, *, #6376, .F. ) ;
#10281 = VERTEX_POINT ( 'NONE', #7881 ) ;
#10282 = EDGE_CURVE ( 'NONE', #8423, #5649, #6554, .T. ) ;
#10283 = DIRECTION ( 'NONE',  ( -1.000000000000000000, 0.000000000000000000, 0.000000000000000000 ) ) ;
#10284 = ORIENTED_EDGE ( 'NONE', *, *, #936, .T. ) ;
#10285 = EDGE_LOOP ( 'NONE', ( #17517, #14141, #6881, #20875 ) ) ;
#10286 = ORIENTED_EDGE ( 'NONE', *, *, #10037, .T. ) ;
#10287 = ADVANCED_FACE ( 'NONE', ( #9741 ), #16381, .F. ) ;
#10288 = LINE ( 'NONE', #5537, #13322 ) ;
#10289 = ORIENTED_EDGE ( 'NONE', *, *, #3701, .T. ) ;
#10290 = DIRECTION ( 'NONE',  ( -1.000000000000000000, -0.000000000000000000, 0.000000000000000000 ) ) ;
#10291 = ADVANCED_FACE ( 'NONE', ( #4784 ), #12736, .F. ) ;
#10292 = DIRECTION ( 'NONE',  ( -1.000000000000000000, 0.000000000000000000, 0.000000000000000000 ) ) ;
#10293 = DIRECTION ( 'NONE',  ( 1.000000000000000000, -0.000000000000000000, -0.000000000000000000 ) ) ;
#10294 = DIRECTION ( 'NONE',  ( 1.000000000000000000, 0.000000000000000000, 0.000000000000000000 ) ) ;
#10295 = CARTESIAN_POINT ( 'NONE',  ( 10.00000000000000000, -52.96496548042899377, 66.55750800669339640 ) ) ;
#10296 = FACE_OUTER_BOUND ( 'NONE', #18535, .T. ) ;
#10297 = CARTESIAN_POINT ( 'NONE',  ( 0.000000000000000000, 27.07404830566971299, 4.815694066514526028 ) ) ;
#10298 = EDGE_CURVE ( 'NONE', #15579, #9606, #12888, .T. ) ;
#10299 = EDGE_LOOP ( 'NONE', ( #16069, #4146, #12218, #9777 ) ) ;
#10300 = CYLINDRICAL_SURFACE ( 'NONE', #7701, 44.99999999999999289 ) ;
#10301 = DIRECTION ( 'NONE',  ( 0.000000000000000000, 0.000000000000000000, 1.000000000000000000 ) ) ;
#10302 = ORIENTED_EDGE ( 'NONE', *, *, #342, .F. ) ;
#10303 = CYLINDRICAL_SURFACE ( 'NONE', #21360, 45.00000000000000000 ) ;
#10304 = ADVANCED_FACE ( 'NONE', ( #3123 ), #9858, .T. ) ;
#10305 = ORIENTED_EDGE ( 'NONE', *, *, #16491, .T. ) ;
#10306 = EDGE_LOOP ( 'NONE', ( #17250, #10772, #13048, #10305 ) ) ;
#10307 = CARTESIAN_POINT ( 'NONE',  ( 10.00000000000000000, 0.000000000000000000, 0.000000000000000000 ) ) ;
#10308 = VERTEX_POINT ( 'NONE', #16495 ) ;
#10309 = ORIENTED_EDGE ( 'NONE', *, *, #19459, .T. ) ;
#10310 = EDGE_CURVE ( 'NONE', #11054, #15560, #18187, .T. ) ;
#10311 = DIRECTION ( 'NONE',  ( 0.000000000000000000, 0.000000000000000000, 1.000000000000000000 ) ) ;
#10312 = CARTESIAN_POINT ( 'NONE',  ( 10.00000000000000000, 0.000000000000000000, 0.000000000000000000 ) ) ;
#10313 = EDGE_CURVE ( 'NONE', #19086, #7932, #16775, .T. ) ;
#10314 = AXIS2_PLACEMENT_3D ( 'NONE', #11494, #4862, #16795 ) ;
#10315 = CARTESIAN_POINT ( 'NONE',  ( 10.00000000000000000, -17.64925110578526812, 86.21197095186339254 ) ) ;
#10316 = DIRECTION ( 'NONE',  ( -1.000000000000000000, 0.000000000000000000, 0.000000000000000000 ) ) ;
#10317 = CARTESIAN_POINT ( 'NONE',  ( 7.999999999999979572, 0.000000000000000000, 0.000000000000000000 ) ) ;
#10318 = DIRECTION ( 'NONE',  ( 0.000000000000000000, -0.5299192642332118952, 0.8480480961564216269 ) ) ;
#10319 = CIRCLE ( 'NONE', #11026, 45.00000000000000000 ) ;
#10320 = CYLINDRICAL_SURFACE ( 'NONE', #3646, 6.887500000000022382 ) ;
#10321 = CARTESIAN_POINT ( 'NONE',  ( 10.00000000000000000, 14.53731623274961571, -23.34226719384889748 ) ) ;
#10322 = ORIENTED_EDGE ( 'NONE', *, *, #21593, .T. ) ;
#10323 = DIRECTION ( 'NONE',  ( -1.000000000000000000, 0.000000000000000000, 0.000000000000000000 ) ) ;
#10324 = AXIS2_PLACEMENT_3D ( 'NONE', #16578, #8182, #14913 ) ;
#10325 = DIRECTION ( 'NONE',  ( 1.000000000000000000, 0.000000000000000000, 0.000000000000000000 ) ) ;
#10326 = EDGE_LOOP ( 'NONE', ( #19436, #17789, #13748, #2642 ) ) ;
#10327 = DIRECTION ( 'NONE',  ( -1.000000000000000000, -0.000000000000000000, 0.000000000000000000 ) ) ;
#10328 = EDGE_LOOP ( 'NONE', ( #6063, #8910 ) ) ;
#10329 = CIRCLE ( 'NONE', #7858, 88.00000000000000000 ) ;
#10330 = DIRECTION ( 'NONE',  ( 1.000000000000000000, 0.000000000000000000, 0.000000000000000000 ) ) ;
#10331 = DIRECTION ( 'NONE',  ( -1.000000000000000000, -0.000000000000000000, 0.000000000000000000 ) ) ;
#10332 = VERTEX_POINT ( 'NONE', #20248 ) ;
#10333 = CIRCLE ( 'NONE', #19155, 92.50100000000000477 ) ;
#10334 = LINE ( 'NONE', #18853, #1089 ) ;
#10335 = ORIENTED_EDGE ( 'NONE', *, *, #9722, .T. ) ;
#10336 = ORIENTED_EDGE ( 'NONE', *, *, #8197, .T. ) ;
#10337 = ORIENTED_EDGE ( 'NONE', *, *, #5001, .F. ) ;
#10338 = DIRECTION ( 'NONE',  ( 1.000000000000000000, 0.000000000000000000, 0.000000000000000000 ) ) ;
#10339 = ORIENTED_EDGE ( 'NONE', *, *, #445, .F. ) ;
#10340 = FACE_OUTER_BOUND ( 'NONE', #10546, .T. ) ;
#10341 = CIRCLE ( 'NONE', #21640, 44.99999999999998579 ) ;
#10342 = DIRECTION ( 'NONE',  ( -1.000000000000000000, 0.000000000000000000, 0.000000000000000000 ) ) ;
#10343 = DIRECTION ( 'NONE',  ( 0.000000000000000000, -1.788692650784974777E-14, -1.000000000000000000 ) ) ;
#10344 = DIRECTION ( 'NONE',  ( 0.000000000000000000, 0.000000000000000000, 1.000000000000000000 ) ) ;
#10345 = CARTESIAN_POINT ( 'NONE',  ( 10.00000000000000000, 22.77465461094694632, -15.41136296218063428 ) ) ;
#10346 = CARTESIAN_POINT ( 'NONE',  ( -1.129531546211690385, 0.000000000000000000, 0.000000000000000000 ) ) ;
#10347 = CIRCLE ( 'NONE', #11405, 88.00000000000000000 ) ;
#10348 = FACE_OUTER_BOUND ( 'NONE', #13074, .T. ) ;
#10349 = DIRECTION ( 'NONE',  ( 0.000000000000000000, 0.000000000000000000, 1.000000000000000000 ) ) ;
#10350 = ORIENTED_EDGE ( 'NONE', *, *, #6090, .T. ) ;
#10351 = CIRCLE ( 'NONE', #11055, 103.6250000000000284 ) ;
#10352 = DIRECTION ( 'NONE',  ( 0.000000000000000000, 0.000000000000000000, 1.000000000000000000 ) ) ;
#10353 = DIRECTION ( 'NONE',  ( 0.000000000000000000, 0.000000000000000000, 1.000000000000000000 ) ) ;
#10354 = CYLINDRICAL_SURFACE ( 'NONE', #8023, 92.50100000000000477 ) ;
#10355 = VERTEX_POINT ( 'NONE', #4997 ) ;
#10356 = ORIENTED_EDGE ( 'NONE', *, *, #21369, .T. ) ;
#10357 = DIRECTION ( 'NONE',  ( 0.000000000000000000, 0.5299192642331997938, 0.8480480961564290654 ) ) ;
#10358 = EDGE_LOOP ( 'NONE', ( #7814, #2760, #3980, #19604 ) ) ;
#10359 = CIRCLE ( 'NONE', #2605, 120.0000000000000000 ) ;
#10360 = ORIENTED_EDGE ( 'NONE', *, *, #16484, .F. ) ;
#10361 = EDGE_CURVE ( 'NONE', #14927, #15756, #1897, .T. ) ;
#10362 = CIRCLE ( 'NONE', #18139, 11.99999999999999822 ) ;
#10363 = ORIENTED_EDGE ( 'NONE', *, *, #456, .T. ) ;
#10364 = DIRECTION ( 'NONE',  ( -1.000000000000000000, -0.000000000000000000, -0.000000000000000000 ) ) ;
#10365 = SHAPE_REPRESENTATION ( 'instrument roller bearing_iso_ISO 1224 - 171015 - R,24,SI,NC,24', ( #15567 ), #4640 ) ;
#10366 = ORIENTED_EDGE ( 'NONE', *, *, #3916, .F. ) ;
#10367 = DIRECTION ( 'NONE',  ( -0.000000000000000000, -0.000000000000000000, -1.000000000000000000 ) ) ;
#10368 = DIRECTION ( 'NONE',  ( 1.000000000000000000, 0.000000000000000000, -0.000000000000000000 ) ) ;
#10369 =( NAMED_UNIT ( * ) PLANE_ANGLE_UNIT ( ) SI_UNIT ( $, .RADIAN. ) );
#10370 = ADVANCED_FACE ( 'NONE', ( #21790, #3225 ), #1688, .T. ) ;
#10371 = AXIS2_PLACEMENT_3D ( 'NONE', #14077, #601, #6023 ) ;
#10372 = DIRECTION ( 'NONE',  ( 0.000000000000000000, 2.775557561562891351E-15, -1.000000000000000000 ) ) ;
#10373 = DIRECTION ( 'NONE',  ( 0.000000000000000000, 0.000000000000000000, -1.000000000000000000 ) ) ;
#10374 = CARTESIAN_POINT ( 'NONE',  ( -5.000000000000000000, 70.00000000000000000, 9.999999999999998224 ) ) ;
#10375 = LINE ( 'NONE', #10490, #604 ) ;
#10376 = DIRECTION ( 'NONE',  ( 0.000000000000000000, 0.000000000000000000, 1.000000000000000000 ) ) ;
#10377 = AXIS2_PLACEMENT_3D ( 'NONE', #14103, #15874, #2271 ) ;
#10378 = ORIENTED_EDGE ( 'NONE', *, *, #7064, .F. ) ;
#10379 = AXIS2_PLACEMENT_3D ( 'NONE', #16960, #53, #14958 ) ;
#10380 = CYLINDRICAL_SURFACE ( 'NONE', #12208, 92.50100000000000477 ) ;
#10381 = ORIENTED_EDGE ( 'NONE', *, *, #16700, .F. ) ;
#10382 = ORIENTED_EDGE ( 'NONE', *, *, #19273, .F. ) ;
#10383 = DIRECTION ( 'NONE',  ( 1.000000000000000000, -0.000000000000000000, -0.000000000000000000 ) ) ;
#10384 = ORIENTED_EDGE ( 'NONE', *, *, #13784, .F. ) ;
#10385 = EDGE_CURVE ( 'NONE', #14091, #10683, #9958, .T. ) ;
#10387 = EDGE_CURVE ( 'NONE', #13415, #4660, #13282, .T. ) ;
#10386 = AXIS2_PLACEMENT_3D ( 'NONE', #6843, #12123, #10581 ) ;
#10388 = EDGE_CURVE ( 'NONE', #11272, #19710, #10061, .T. ) ;
#10389 = AXIS2_PLACEMENT_3D ( 'NONE', #20577, #3890, #20369 ) ;
#10390 = VERTEX_POINT ( 'NONE', #15368 ) ;
#10391 = VECTOR ( 'NONE', #7447, 1000.000000000000000 ) ;
#10392 = CYLINDRICAL_SURFACE ( 'NONE', #19680, 92.50100000000000477 ) ;
#10393 = EDGE_CURVE ( 'NONE', #4335, #6526, #11733, .T. ) ;
#10394 = EDGE_LOOP ( 'NONE', ( #10066, #5722, #6610, #12505 ) ) ;
#10395 = CIRCLE ( 'NONE', #21348, 5.000000000000000888 ) ;
#10396 = CARTESIAN_POINT ( 'NONE',  ( 10.00000000000000000, 0.000000000000000000, 0.000000000000000000 ) ) ;
#10397 = FACE_OUTER_BOUND ( 'NONE', #7924, .T. ) ;
#10398 = DIRECTION ( 'NONE',  ( -1.000000000000000000, -0.000000000000000000, -0.000000000000000000 ) ) ;
#10399 = DIRECTION ( 'NONE',  ( 0.000000000000000000, 0.000000000000000000, 1.000000000000000000 ) ) ;
#10400 = DIRECTION ( 'NONE',  ( -0.000000000000000000, -1.000000000000000000, -0.000000000000000000 ) ) ;
#10401 = DIRECTION ( 'NONE',  ( -1.000000000000000000, -0.000000000000000000, 0.000000000000000000 ) ) ;
#10402 = EDGE_CURVE ( 'NONE', #3628, #9187, #6884, .T. ) ;
#10403 = CYLINDRICAL_SURFACE ( 'NONE', #10866, 92.50100000000000477 ) ;
#10404 = CIRCLE ( 'NONE', #16398, 88.00000000000000000 ) ;
#10405 = AXIS2_PLACEMENT_3D ( 'NONE', #2280, #19300, #17873 ) ;
#10406 = EDGE_LOOP ( 'NONE', ( #9392, #13515, #3739, #18496 ) ) ;
#10407 = EDGE_CURVE ( 'NONE', #4687, #3326, #3712, .T. ) ;
#10408 = AXIS2_PLACEMENT_3D ( 'NONE', #2805, #2902, #12840 ) ;
#10409 = CIRCLE ( 'NONE', #12180, 44.99999999999998579 ) ;
#10410 = LINE ( 'NONE', #13621, #17579 ) ;
#10411 = LINE ( 'NONE', #14158, #9167 ) ;
#10412 = VERTEX_POINT ( 'NONE', #20033 ) ;
#10413 = CIRCLE ( 'NONE', #6922, 11.99999999999999822 ) ;
#10414 = DIRECTION ( 'NONE',  ( 0.000000000000000000, 1.850371707708594760E-15, -1.000000000000000000 ) ) ;
#10415 = ORIENTED_EDGE ( 'NONE', *, *, #17562, .T. ) ;
#10416 = SURFACE_SIDE_STYLE ('',( #12297 ) ) ;
#10417 = ORIENTED_EDGE ( 'NONE', *, *, #14907, .F. ) ;
#10418 = CARTESIAN_POINT ( 'NONE',  ( 10.00000000000000000, 0.000000000000000000, 0.000000000000000000 ) ) ;
#10419 = EDGE_CURVE ( 'NONE', #4590, #3028, #18553, .T. ) ;
#10420 = ORIENTED_EDGE ( 'NONE', *, *, #7042, .T. ) ;
#10421 = AXIS2_PLACEMENT_3D ( 'NONE', #12933, #6002, #21015 ) ;
#10422 = EDGE_LOOP ( 'NONE', ( #19252, #13653, #11427, #2708 ) ) ;
#10423 = DIRECTION ( 'NONE',  ( 0.000000000000000000, 0.000000000000000000, -1.000000000000000000 ) ) ;
#10424 = DIRECTION ( 'NONE',  ( 1.000000000000000000, 0.000000000000000000, 0.000000000000000000 ) ) ;
#10425 = CIRCLE ( 'NONE', #9362, 44.99999999999999289 ) ;
#10426 = AXIS2_PLACEMENT_3D ( 'NONE', #20711, #1823, #8560 ) ;
#10427 = LINE ( 'NONE', #5356, #11456 ) ;
#10428 = DIRECTION ( 'NONE',  ( -1.000000000000000000, -0.000000000000000000, -0.000000000000000000 ) ) ;
#10429 = CARTESIAN_POINT ( 'NONE',  ( 10.00000000000000000, -78.04699792498179534, 49.64978465107262906 ) ) ;
#10430 = CYLINDRICAL_SURFACE ( 'NONE', #14962, 92.50100000000000477 ) ;
#10431 = CARTESIAN_POINT ( 'NONE',  ( 0.000000000000000000, -0.6021240089799234640, -31.99433460282945063 ) ) ;
#10432 = DIRECTION ( 'NONE',  ( -1.000000000000000000, 0.000000000000000000, -0.000000000000000000 ) ) ;
#10433 = ADVANCED_FACE ( 'NONE', ( #15052 ), #6992, .F. ) ;
#10434 = ORIENTED_EDGE ( 'NONE', *, *, #18545, .T. ) ;
#10435 = ADVANCED_FACE ( 'NONE', ( #14939 ), #15159, .F. ) ;
#10436 = CARTESIAN_POINT ( 'NONE',  ( 10.00000000000000000, 24.73395913766480447, -12.01774797440553044 ) ) ;
#10437 = ORIENTED_EDGE ( 'NONE', *, *, #842, .T. ) ;
#10438 = AXIS2_PLACEMENT_3D ( 'NONE', #17076, #2454, #15412 ) ;
#10439 = EDGE_CURVE ( 'NONE', #20835, #5395, #20999, .T. ) ;
#10440 = CIRCLE ( 'NONE', #7970, 27.49900000000000944 ) ;
#10441 = VECTOR ( 'NONE', #20146, 1000.000000000000000 ) ;
#10442 = ADVANCED_FACE ( 'NONE', ( #10397 ), #6779, .T. ) ;
#10443 = CARTESIAN_POINT ( 'NONE',  ( 0.000000000000000000, 79.38136668499741688, 37.98155635597341728 ) ) ;
#10444 = AXIS2_PLACEMENT_3D ( 'NONE', #3992, #5882, #2338 ) ;
#10445 = ORIENTED_EDGE ( 'NONE', *, *, #20284, .F. ) ;
#10446 = DIRECTION ( 'NONE',  ( -1.000000000000000000, 0.000000000000000000, -0.000000000000000000 ) ) ;
#10447 = CYLINDRICAL_SURFACE ( 'NONE', #16919, 12.00000000000000000 ) ;
#10448 = ORIENTED_EDGE ( 'NONE', *, *, #2425, .T. ) ;
#10449 = VERTEX_POINT ( 'NONE', #20474 ) ;
#10450 = EDGE_CURVE ( 'NONE', #7150, #21231, #13608, .T. ) ;
#10451 = ORIENTED_EDGE ( 'NONE', *, *, #14581, .F. ) ;
#10452 = ORIENTED_EDGE ( 'NONE', *, *, #9189, .T. ) ;
#10453 = DIRECTION ( 'NONE',  ( 0.000000000000000000, 0.000000000000000000, 1.000000000000000000 ) ) ;
#10454 = VERTEX_POINT ( 'NONE', #17039 ) ;
#10455 = CARTESIAN_POINT ( 'NONE',  ( -10.00000000000000000, 0.000000000000000000, 0.000000000000000000 ) ) ;
#10456 = DIRECTION ( 'NONE',  ( -1.000000000000000000, -0.000000000000000000, -0.000000000000000000 ) ) ;
#10457 = FACE_OUTER_BOUND ( 'NONE', #10231, .T. ) ;
#10458 = CIRCLE ( 'NONE', #13625, 11.99999999999999822 ) ;
#10459 = CARTESIAN_POINT ( 'NONE',  ( 0.000000000000000000, 0.000000000000000000, 0.000000000000000000 ) ) ;
#10460 = CARTESIAN_POINT ( 'NONE',  ( 5.000000000000000000, 12.46320060045723999, 29.47318494484033025 ) ) ;
#10461 = AXIS2_PLACEMENT_3D ( 'NONE', #11499, #6207, #6433 ) ;
#10462 = CARTESIAN_POINT ( 'NONE',  ( 0.000000000000000000, -75.87763420127865288, 44.57111876559696384 ) ) ;
#10463 = DIRECTION ( 'NONE',  ( -1.000000000000000000, -0.000000000000000000, -0.000000000000000000 ) ) ;
#10464 = DIRECTION ( 'NONE',  ( 0.000000000000000000, 0.000000000000000000, 1.000000000000000000 ) ) ;
#10465 = EDGE_LOOP ( 'NONE', ( #4412, #17248, #6449, #14610 ) ) ;
#10466 = DIRECTION ( 'NONE',  ( -1.000000000000000000, -0.000000000000000000, 0.000000000000000000 ) ) ;
#10467 = LINE ( 'NONE', #15326, #8994 ) ;
#10468 = DIRECTION ( 'NONE',  ( 1.000000000000000000, 0.000000000000000000, 0.000000000000000000 ) ) ;
#10469 = VERTEX_POINT ( 'NONE', #12059 ) ;
#10470 = VECTOR ( 'NONE', #1550, 1000.000000000000000 ) ;
#10472 = CIRCLE ( 'NONE', #16466, 44.99999999999999289 ) ;
#10471 = FACE_OUTER_BOUND ( 'NONE', #11686, .T. ) ;
#10473 = AXIS2_PLACEMENT_3D ( 'NONE', #11700, #10026, #19988 ) ;
#10474 = EDGE_LOOP ( 'NONE', ( #13815, #14245, #14417, #13535 ) ) ;
#10475 = CARTESIAN_POINT ( 'NONE',  ( 5.000000000000000000, -78.80192417387952730, 39.16958956249271040 ) ) ;
#10476 = VERTEX_POINT ( 'NONE', #3663 ) ;
#10477 = EDGE_LOOP ( 'NONE', ( #7191, #1734, #17665, #9926 ) ) ;
#10478 = EDGE_LOOP ( 'NONE', ( #16127, #848, #15097, #18321 ) ) ;
#10479 = CARTESIAN_POINT ( 'NONE',  ( -10.00000000000000000, 0.000000000000000000, 0.000000000000000000 ) ) ;
#10480 = DIRECTION ( 'NONE',  ( 0.000000000000000000, -0.9510565162951503115, -0.3090169943749573878 ) ) ;
#10481 = CARTESIAN_POINT ( 'NONE',  ( 0.000000000000000000, -84.80486432185169576, -36.94008646920480743 ) ) ;
#10482 = CYLINDRICAL_SURFACE ( 'NONE', #12793, 3.000000000000000000 ) ;
#10483 = UNCERTAINTY_MEASURE_WITH_UNIT (LENGTH_MEASURE( 1.000000000000000082E-05 ), #9517, 'distance_accuracy_value', 'NONE');
#10484 = CIRCLE ( 'NONE', #19666, 44.99999999999999289 ) ;
#10485 = CYLINDRICAL_SURFACE ( 'NONE', #15266, 44.99999999999999289 ) ;
#10486 = CIRCLE ( 'NONE', #10125, 92.50100000000000477 ) ;
#10487 = DIRECTION ( 'NONE',  ( 0.000000000000000000, 0.000000000000000000, 1.000000000000000000 ) ) ;
#10488 = CARTESIAN_POINT ( 'NONE',  ( -5.000000000000000000, 5.000000000000000000, 15.00000000000000000 ) ) ;
#10489 = AXIS2_PLACEMENT_3D ( 'NONE', #15322, #16768, #11801 ) ;
#10490 = CARTESIAN_POINT ( 'NONE',  ( -1.500000000000000000, -4.769696007084728073, 100.0000000000000000 ) ) ;
#10491 = DIRECTION ( 'NONE',  ( -1.000000000000000000, 0.000000000000000000, -0.000000000000000000 ) ) ;
#10492 = EDGE_CURVE ( 'NONE', #12605, #4009, #17151, .T. ) ;
#10493 = ORIENTED_EDGE ( 'NONE', *, *, #19905, .F. ) ;
#10494 = CARTESIAN_POINT ( 'NONE',  ( 0.000000000000000000, 0.000000000000000000, 3.000000000000000000 ) ) ;
#10495 = EDGE_LOOP ( 'NONE', ( #853, #15182 ) ) ;
#10496 = ORIENTED_EDGE ( 'NONE', *, *, #9205, .F. ) ;
#10497 = EDGE_CURVE ( 'NONE', #6423, #10755, #10834, .T. ) ;
#10498 = VERTEX_POINT ( 'NONE', #4103 ) ;
#10499 = CIRCLE ( 'NONE', #3459, 44.99999999999999289 ) ;
#10500 = CARTESIAN_POINT ( 'NONE',  ( 1.500000000000000000, 5.000000000000000000, 0.000000000000000000 ) ) ;
#10501 = ORIENTED_EDGE ( 'NONE', *, *, #10962, .F. ) ;
#10502 = AXIS2_PLACEMENT_3D ( 'NONE', #15642, #513, #7261 ) ;
#10503 = VERTEX_POINT ( 'NONE', #17480 ) ;
#10504 = CIRCLE ( 'NONE', #21452, 32.00000000000000000 ) ;
#10505 = CARTESIAN_POINT ( 'NONE',  ( 10.00000000000000000, 39.87723064937233630, -83.46401306393528330 ) ) ;
#10506 = ORIENTED_EDGE ( 'NONE', *, *, #10568, .T. ) ;
#10507 = DIRECTION ( 'NONE',  ( -1.000000000000000000, 0.000000000000000000, 0.000000000000000000 ) ) ;
#10508 = CARTESIAN_POINT ( 'NONE',  ( 10.00000000000000000, 9.992993448021948666, -26.36019881529875519 ) ) ;
#10509 = DIRECTION ( 'NONE',  ( -1.000000000000000000, -0.000000000000000000, 0.000000000000000000 ) ) ;
#10510 = CARTESIAN_POINT ( 'NONE',  ( 10.00000000000000000, 91.49386717542222414, 13.61276130277023810 ) ) ;
#10511 = CARTESIAN_POINT ( 'NONE',  ( 9.999999999999998224, 1.224646799147353059E-15, 3.000000000000000000 ) ) ;
#10512 = FACE_OUTER_BOUND ( 'NONE', #11561, .T. ) ;
#10513 = CARTESIAN_POINT ( 'NONE',  ( 10.00000000000000000, 0.000000000000000000, 0.000000000000000000 ) ) ;
#10514 = CIRCLE ( 'NONE', #18997, 44.99999999999999289 ) ;
#10515 = AXIS2_PLACEMENT_3D ( 'NONE', #2246, #5357, #383 ) ;
#10516 = ADVANCED_FACE ( 'NONE', ( #14045 ), #15703, .T. ) ;
#10517 = AXIS2_PLACEMENT_3D ( 'NONE', #4116, #17496, #2669 ) ;
#10518 = ORIENTED_EDGE ( 'NONE', *, *, #17021, .T. ) ;
#10519 = CIRCLE ( 'NONE', #5960, 44.99999999999999289 ) ;
#10520 = LINE ( 'NONE', #3349, #16168 ) ;
#10521 = CARTESIAN_POINT ( 'NONE',  ( -90.00000000000000000, 0.000000000000000000, 0.000000000000000000 ) ) ;
#10522 = ORIENTED_EDGE ( 'NONE', *, *, #10676, .F. ) ;
#10523 = FACE_OUTER_BOUND ( 'NONE', #7835, .T. ) ;
#10524 = ORIENTED_EDGE ( 'NONE', *, *, #5811, .F. ) ;
#10525 = EDGE_CURVE ( 'NONE', #14824, #1075, #9066, .T. ) ;
#10526 = AXIS2_PLACEMENT_3D ( 'NONE', #20863, #12572, #5732 ) ;
#10527 = CARTESIAN_POINT ( 'NONE',  ( 1.500000000000001332, 0.000000000000000000, 0.000000000000000000 ) ) ;
#10528 = VERTEX_POINT ( 'NONE', #8956 ) ;
#10529 = AXIS2_PLACEMENT_3D ( 'NONE', #10735, #900, #9078 ) ;
#10530 = ORIENTED_EDGE ( 'NONE', *, *, #19205, .T. ) ;
#10531 = AXIS2_PLACEMENT_3D ( 'NONE', #11498, #1110, #4648 ) ;
#10532 = DIRECTION ( 'NONE',  ( 1.000000000000000000, 0.000000000000000000, 0.000000000000000000 ) ) ;
#10533 = VECTOR ( 'NONE', #13350, 1000.000000000000000 ) ;
#10534 = CARTESIAN_POINT ( 'NONE',  ( 5.000000000000000000, -75.87763420127865288, 44.57111876559696384 ) ) ;
#10535 = AXIS2_PLACEMENT_3D ( 'NONE', #7731, #14133, #10812 ) ;
#10536 = EDGE_CURVE ( 'NONE', #9780, #17002, #4421, .T. ) ;
#10537 = LINE ( 'NONE', #10860, #19217 ) ;
#10538 = CARTESIAN_POINT ( 'NONE',  ( 5.000000000000000000, -13.56333590714035253, 28.98337314858430602 ) ) ;
#10539 = DIRECTION ( 'NONE',  ( 0.000000000000000000, -3.376928366568185319E-14, -1.000000000000000000 ) ) ;
#10540 = DIRECTION ( 'NONE',  ( 1.000000000000000000, 0.000000000000000000, 0.000000000000000000 ) ) ;
#10541 = CARTESIAN_POINT ( 'NONE',  ( 10.00000000000000000, 26.69209308833516658, -6.612652082459054448 ) ) ;
#10542 = DIRECTION ( 'NONE',  ( 0.000000000000000000, 0.000000000000000000, -1.000000000000000000 ) ) ;
#10543 = EDGE_CURVE ( 'NONE', #5699, #17767, #21367, .T. ) ;
#10544 = ADVANCED_FACE ( 'NONE', ( #12169 ), #17264, .T. ) ;
#10545 = ADVANCED_FACE ( 'NONE', ( #10725 ), #5141, .T. ) ;
#10546 = EDGE_LOOP ( 'NONE', ( #4968, #907, #12300, #18090 ) ) ;
#10547 = DIRECTION ( 'NONE',  ( 0.000000000000000000, 0.000000000000000000, -1.000000000000000000 ) ) ;
#10548 = CIRCLE ( 'NONE', #13735, 88.00000000000000000 ) ;
#10549 = EDGE_CURVE ( 'NONE', #19408, #1529, #17475, .T. ) ;
#10550 = AXIS2_PLACEMENT_3D ( 'NONE', #15307, #2157, #13867 ) ;
#10551 = ORIENTED_EDGE ( 'NONE', *, *, #14057, .T. ) ;
#10552 = VECTOR ( 'NONE', #10030, 1000.000000000000000 ) ;
#10553 = CIRCLE ( 'NONE', #5612, 88.00000000000000000 ) ;
#10554 = CARTESIAN_POINT ( 'NONE',  ( 10.00000000000000000, 0.000000000000000000, 0.000000000000000000 ) ) ;
#10555 = ORIENTED_EDGE ( 'NONE', *, *, #4967, .F. ) ;
#10556 = DIRECTION ( 'NONE',  ( -1.000000000000000000, 0.000000000000000000, 0.000000000000000000 ) ) ;
#10557 = DIRECTION ( 'NONE',  ( 0.000000000000000000, 0.000000000000000000, 1.000000000000000000 ) ) ;
#10558 = ORIENTED_EDGE ( 'NONE', *, *, #144, .T. ) ;
#10559 = SURFACE_STYLE_USAGE ( .BOTH. , #12535 ) ;
#10560 = EDGE_CURVE ( 'NONE', #5306, #15511, #1948, .T. ) ;
#10561 = VERTEX_POINT ( 'NONE', #10618 ) ;
#10562 = EDGE_LOOP ( 'NONE', ( #4683, #2161, #7408, #1291 ) ) ;
#10563 = ORIENTED_EDGE ( 'NONE', *, *, #3671, .T. ) ;
#10564 = DIRECTION ( 'NONE',  ( -1.000000000000000000, 0.000000000000000000, 0.000000000000000000 ) ) ;
#10565 = AXIS2_PLACEMENT_3D ( 'NONE', #140, #6888, #7107 ) ;
#10566 = ADVANCED_FACE ( 'NONE', ( #12597 ), #12381, .F. ) ;
#10567 = ORIENTED_EDGE ( 'NONE', *, *, #13808, .F. ) ;
#10568 = EDGE_CURVE ( 'NONE', #4414, #21336, #7320, .T. ) ;
#10569 = AXIS2_PLACEMENT_3D ( 'NONE', #3452, #8530, #1687 ) ;
#10570 = DIRECTION ( 'NONE',  ( -1.000000000000000000, 0.000000000000000000, -0.000000000000000000 ) ) ;
#10571 = FACE_OUTER_BOUND ( 'NONE', #1532, .T. ) ;
#10572 = DIRECTION ( 'NONE',  ( 0.000000000000000000, 0.5877852522924742473, -0.8090169943749465631 ) ) ;
#10573 = VECTOR ( 'NONE', #4048, 1000.000000000000000 ) ;
#10574 = DIRECTION ( 'NONE',  ( -1.000000000000000000, -0.000000000000000000, -0.000000000000000000 ) ) ;
#10575 = EDGE_CURVE ( 'NONE', #7569, #20616, #2999, .T. ) ;
#10576 = CARTESIAN_POINT ( 'NONE',  ( 10.00000000000000000, 84.80486432185190893, 36.94008646920423899 ) ) ;
#10577 = CARTESIAN_POINT ( 'NONE',  ( 10.00000000000000000, -9.992993448021419312, -26.36019881529895770 ) ) ;
#10578 = ORIENTED_EDGE ( 'NONE', *, *, #2028, .F. ) ;
#10579 = DIRECTION ( 'NONE',  ( 0.000000000000000000, 0.9702957262759972501, -0.2419218955996649267 ) ) ;
#10580 = EDGE_CURVE ( 'NONE', #13685, #21761, #4054, .T. ) ;
#10581 = DIRECTION ( 'NONE',  ( 0.000000000000000000, 0.8660254037844398178, -0.4999999999999979461 ) ) ;
#10582 = DIRECTION ( 'NONE',  ( -1.000000000000000000, 0.000000000000000000, -0.000000000000000000 ) ) ;
#10583 = ORIENTED_EDGE ( 'NONE', *, *, #10930, .T. ) ;
#10584 = CARTESIAN_POINT ( 'NONE',  ( 10.00000000000000000, -19.07277123396528395, -19.80970465344768172 ) ) ;
#10585 = ORIENTED_EDGE ( 'NONE', *, *, #552, .T. ) ;
#10586 = MECHANICAL_DESIGN_GEOMETRIC_PRESENTATION_REPRESENTATION (  '', ( #9156 ), #12693 ) ;
#10587 = DIRECTION ( 'NONE',  ( -1.000000000000000000, 0.000000000000000000, -0.000000000000000000 ) ) ;
#10588 = ORIENTED_EDGE ( 'NONE', *, *, #13906, .F. ) ;
#10589 = ORIENTED_EDGE ( 'NONE', *, *, #8777, .F. ) ;
#10590 = CARTESIAN_POINT ( 'NONE',  ( 0.000000000000000000, 0.000000000000000000, 25.00000000000000000 ) ) ;
#10591 = EDGE_CURVE ( 'NONE', #5623, #13276, #9702, .T. ) ;
#10592 = ORIENTED_EDGE ( 'NONE', *, *, #5811, .T. ) ;
#10593 = CARTESIAN_POINT ( 'NONE',  ( -140.0000507999999968, 4.000000000000000000, -1.000000000000000000 ) ) ;
#10594 = CARTESIAN_POINT ( 'NONE',  ( 0.000000000000000000, -89.12061559554315693, -24.77803214283632371 ) ) ;
#10595 = DIRECTION ( 'NONE',  ( 1.000000000000000000, 0.000000000000000000, 0.000000000000000000 ) ) ;
#10596 = DIRECTION ( 'NONE',  ( -1.000000000000000000, -0.000000000000000000, -0.000000000000000000 ) ) ;
#10597 = ADVANCED_FACE ( 'NONE', ( #2332 ), #4078, .T. ) ;
#10598 = LINE ( 'NONE', #2102, #800 ) ;
#10599 = CARTESIAN_POINT ( 'NONE',  ( 0.000000000000000000, -19.29292659244022801, 25.53004080487755800 ) ) ;
#10600 = LINE ( 'NONE', #10488, #19565 ) ;
#10601 = CIRCLE ( 'NONE', #9888, 45.00000000000000711 ) ;
#10602 = DIRECTION ( 'NONE',  ( 1.000000000000000000, 0.000000000000000000, 0.000000000000000000 ) ) ;
#10603 = CARTESIAN_POINT ( 'NONE',  ( 10.00000000000000000, 0.000000000000000000, 0.000000000000000000 ) ) ;
#10604 = VERTEX_POINT ( 'NONE', #2011 ) ;
#10605 = DIRECTION ( 'NONE',  ( 0.000000000000000000, 0.000000000000000000, 1.000000000000000000 ) ) ;
#10606 = ORIENTED_EDGE ( 'NONE', *, *, #3518, .T. ) ;
#10607 = ORIENTED_EDGE ( 'NONE', *, *, #10361, .F. ) ;
#10608 = ORIENTED_EDGE ( 'NONE', *, *, #19588, .F. ) ;
#10609 = CARTESIAN_POINT ( 'NONE',  ( 5.000000000000000000, 83.48638250753229784, 27.82128566055142826 ) ) ;
#10610 = ORIENTED_EDGE ( 'NONE', *, *, #20677, .F. ) ;
#10611 = VECTOR ( 'NONE', #10383, 1000.000000000000000 ) ;
#10612 = VERTEX_POINT ( 'NONE', #20888 ) ;
#10613 = EDGE_CURVE ( 'NONE', #49, #5365, #8666, .T. ) ;
#10614 = DIRECTION ( 'NONE',  ( 0.000000000000000000, -0.7880107536067146867, -0.6156614753256676176 ) ) ;
#10615 = ORIENTED_EDGE ( 'NONE', *, *, #5147, .T. ) ;
#10616 = DIRECTION ( 'NONE',  ( 0.000000000000000000, 0.000000000000000000, 1.000000000000000000 ) ) ;
#10617 = CARTESIAN_POINT ( 'NONE',  ( 10.00000000000000000, 90.63195040374210976, -18.50093422002330712 ) ) ;
#10618 = CARTESIAN_POINT ( 'NONE',  ( 0.000000000000000000, -83.48638250753209888, -27.82128566055197538 ) ) ;
#10619 = CARTESIAN_POINT ( 'NONE',  ( 10.00000000000000000, -69.25892805976543798, 49.38005998797819274 ) ) ;
#10620 = LINE ( 'NONE', #12599, #590 ) ;
#10621 = FACE_OUTER_BOUND ( 'NONE', #19177, .T. ) ;
#10622 = LINE ( 'NONE', #13616, #21374 ) ;
#10623 = CYLINDRICAL_SURFACE ( 'NONE', #9805, 11.99999999999999822 ) ;
#10624 = CIRCLE ( 'NONE', #16976, 44.99999999999999289 ) ;
#10625 = EDGE_LOOP ( 'NONE', ( #14221, #5347, #4138, #13251 ) ) ;
#10626 = DIRECTION ( 'NONE',  ( 1.000000000000000000, 0.000000000000000000, 0.000000000000000000 ) ) ;
#10627 = DIRECTION ( 'NONE',  ( 0.000000000000000000, 0.000000000000000000, 1.000000000000000000 ) ) ;
#10628 = EDGE_LOOP ( 'NONE', ( #10909, #1159, #7073, #2229 ) ) ;
#10629 = DIRECTION ( 'NONE',  ( 0.000000000000000000, 0.000000000000000000, -1.000000000000000000 ) ) ;
#10630 = VERTEX_POINT ( 'NONE', #19556 ) ;
#10631 = DIRECTION ( 'NONE',  ( 0.000000000000000000, 0.000000000000000000, 1.000000000000000000 ) ) ;
#10632 = EDGE_LOOP ( 'NONE', ( #8173, #10578 ) ) ;
#10633 = EDGE_CURVE ( 'NONE', #1387, #21723, #20320, .T. ) ;
#10634 = VERTEX_POINT ( 'NONE', #5991 ) ;
#10635 = MECHANICAL_DESIGN_GEOMETRIC_PRESENTATION_REPRESENTATION (  '', ( #17355 ), #1816 ) ;
#10636 = FACE_BOUND ( 'NONE', #18431, .T. ) ;
#10637 = DIRECTION ( 'NONE',  ( -1.000000000000000000, 0.000000000000000000, 0.000000000000000000 ) ) ;
#10638 = LINE ( 'NONE', #15613, #9330 ) ;
#10639 = LINE ( 'NONE', #17392, #4880 ) ;
#10640 = CARTESIAN_POINT ( 'NONE',  ( 0.000000000000000000, 0.000000000000000000, 0.000000000000000000 ) ) ;
#10641 = DIRECTION ( 'NONE',  ( 0.000000000000000000, -0.3420201433256757073, 0.9396926207859058744 ) ) ;
#10642 = EDGE_CURVE ( 'NONE', #12774, #21645, #3025, .T. ) ;
#10643 = AXIS2_PLACEMENT_3D ( 'NONE', #19650, #4625, #9244 ) ;
#10644 = DIRECTION ( 'NONE',  ( 0.000000000000000000, 0.000000000000000000, 1.000000000000000000 ) ) ;
#10645 = LINE ( 'NONE', #280, #19456 ) ;
#10646 = VERTEX_POINT ( 'NONE', #9498 ) ;
#10647 = DIRECTION ( 'NONE',  ( 0.000000000000000000, 0.000000000000000000, 1.000000000000000000 ) ) ;
#10648 = EDGE_CURVE ( 'NONE', #5893, #10454, #4795, .T. ) ;
#10649 = EDGE_LOOP ( 'NONE', ( #9506, #18324, #3069, #21671 ) ) ;
#10650 = DIRECTION ( 'NONE',  ( 0.000000000000000000, -0.5299192642332118952, 0.8480480961564216269 ) ) ;
#10651 = EDGE_LOOP ( 'NONE', ( #904, #764, #3531, #15526 ) ) ;
#10652 = DIRECTION ( 'NONE',  ( 1.000000000000000000, 0.000000000000000000, 0.000000000000000000 ) ) ;
#10653 = AXIS2_PLACEMENT_3D ( 'NONE', #678, #5436, #571 ) ;
#10654 = CARTESIAN_POINT ( 'NONE',  ( 10.00000000000000000, -57.53593069156319473, -72.42963261301021305 ) ) ;
#10655 = ORIENTED_EDGE ( 'NONE', *, *, #14233, .F. ) ;
#10657 = ADVANCED_FACE ( 'NONE', ( #16465 ), #4427, .T. ) ;
#10656 = ORIENTED_EDGE ( 'NONE', *, *, #17335, .T. ) ;
#10658 = CIRCLE ( 'NONE', #19843, 12.00000000000000000 ) ;
#10659 = ORIENTED_EDGE ( 'NONE', *, *, #9812, .T. ) ;
#10660 = ADVANCED_FACE ( 'NONE', ( #1335 ), #19785, .F. ) ;
#10661 = ORIENTED_EDGE ( 'NONE', *, *, #7050, .T. ) ;
#10662 = ADVANCED_FACE ( 'NONE', ( #14586 ), #21323, .F. ) ;
#10663 = DIRECTION ( 'NONE',  ( -0.000000000000000000, -0.000000000000000000, 1.000000000000000000 ) ) ;
#10664 = VECTOR ( 'NONE', #1523, 1000.000000000000000 ) ;
#10665 = ORIENTED_EDGE ( 'NONE', *, *, #4884, .T. ) ;
#10666 = ADVANCED_FACE ( 'NONE', ( #14485 ), #11278, .F. ) ;
#10667 = CARTESIAN_POINT ( 'NONE',  ( 0.000000000000000000, 0.000000000000000000, 0.000000000000000000 ) ) ;
#10668 = CARTESIAN_POINT ( 'NONE',  ( 0.000000000000000000, -25.48117629651196125, 10.33947075754252332 ) ) ;
#10669 = DIRECTION ( 'NONE',  ( -1.000000000000000000, 0.000000000000000000, 0.000000000000000000 ) ) ;
#10670 = DIRECTION ( 'NONE',  ( -1.000000000000000000, -0.000000000000000000, -0.000000000000000000 ) ) ;
#10671 = DIRECTION ( 'NONE',  ( -0.000000000000000000, -0.000000000000000000, -1.000000000000000000 ) ) ;
#10672 = PRESENTATION_LAYER_ASSIGNMENT (  '', '', ( #14569 ) ) ;
#10673 = DIRECTION ( 'NONE',  ( 0.000000000000000000, 0.000000000000000000, 1.000000000000000000 ) ) ;
#10674 = ORIENTED_EDGE ( 'NONE', *, *, #4224, .F. ) ;
#10675 = DIRECTION ( 'NONE',  ( 1.000000000000000000, -0.000000000000000000, -0.000000000000000000 ) ) ;
#10676 = EDGE_CURVE ( 'NONE', #9950, #20418, #21016, .T. ) ;
#10677 = AXIS2_PLACEMENT_3D ( 'NONE', #17014, #109, #1872 ) ;
#10678 = VECTOR ( 'NONE', #17236, 1000.000000000000000 ) ;
#10679 = DIRECTION ( 'NONE',  ( 0.000000000000000000, 0.2079116908177598144, -0.9781476007338055778 ) ) ;
#10680 = CIRCLE ( 'NONE', #21633, 44.99999999999999289 ) ;
#10681 = EDGE_CURVE ( 'NONE', #21786, #827, #10769, .T. ) ;
#10682 = DIRECTION ( 'NONE',  ( 0.000000000000000000, 0.000000000000000000, 1.000000000000000000 ) ) ;
#10683 = VERTEX_POINT ( 'NONE', #21222 ) ;
#10684 = DIRECTION ( 'NONE',  ( -1.000000000000000000, -0.000000000000000000, -0.000000000000000000 ) ) ;
#10685 = VERTEX_POINT ( 'NONE', #17916 ) ;
#10686 = CARTESIAN_POINT ( 'NONE',  ( 10.00000000000000000, 86.66425444033919234, 32.33793443156426406 ) ) ;
#10687 = ORIENTED_EDGE ( 'NONE', *, *, #14313, .F. ) ;
#10688 = AXIS2_PLACEMENT_3D ( 'NONE', #17559, #17775, #12904 ) ;
#10689 = ORIENTED_EDGE ( 'NONE', *, *, #14705, .T. ) ;
#10690 = VERTEX_POINT ( 'NONE', #12924 ) ;
#10691 = DIRECTION ( 'NONE',  ( 0.000000000000000000, 0.000000000000000000, 1.000000000000000000 ) ) ;
#10692 = ORIENTED_EDGE ( 'NONE', *, *, #2082, .F. ) ;
#10693 = DIRECTION ( 'NONE',  ( 0.000000000000000000, 0.000000000000000000, 1.000000000000000000 ) ) ;
#10694 = CIRCLE ( 'NONE', #21282, 11.99999999999999822 ) ;
#10695 = EDGE_CURVE ( 'NONE', #5372, #18178, #19863, .T. ) ;
#10696 = DIRECTION ( 'NONE',  ( 1.000000000000000000, 0.000000000000000000, 0.000000000000000000 ) ) ;
#10697 = DIRECTION ( 'NONE',  ( 0.000000000000000000, 0.000000000000000000, 1.000000000000000000 ) ) ;
#10698 = AXIS2_PLACEMENT_3D ( 'NONE', #13747, #5458, #10631 ) ;
#10699 = CARTESIAN_POINT ( 'NONE',  ( 5.000000000000000888, -18.31866948046748078, -26.23788002993743262 ) ) ;
#10700 = CARTESIAN_POINT ( 'NONE',  ( -8.000000000000007105, 0.000000000000000000, 0.000000000000000000 ) ) ;
#10701 = DIRECTION ( 'NONE',  ( -1.000000000000000000, -0.000000000000000000, -0.000000000000000000 ) ) ;
#10702 = DIRECTION ( 'NONE',  ( -1.000000000000000000, -0.000000000000000000, -0.000000000000000000 ) ) ;
#10703 = CARTESIAN_POINT ( 'NONE',  ( 0.000000000000000000, -29.47587714451095309, 82.91666097089111531 ) ) ;
#10704 = EDGE_CURVE ( 'NONE', #2939, #19686, #1157, .T. ) ;
#10705 = CIRCLE ( 'NONE', #1893, 27.49900000000000233 ) ;
#10706 = ORIENTED_EDGE ( 'NONE', *, *, #3689, .T. ) ;
#10707 = EDGE_CURVE ( 'NONE', #1807, #10390, #3630, .T. ) ;
#10708 = DIRECTION ( 'NONE',  ( -1.000000000000000000, 0.000000000000000000, 0.000000000000000000 ) ) ;
#10709 = VECTOR ( 'NONE', #9745, 1000.000000000000000 ) ;
#10710 = ORIENTED_EDGE ( 'NONE', *, *, #12564, .F. ) ;
#10711 = ORIENTED_EDGE ( 'NONE', *, *, #10575, .F. ) ;
#10712 = EDGE_CURVE ( 'NONE', #1586, #7680, #1222, .T. ) ;
#10713 = AXIS2_PLACEMENT_3D ( 'NONE', #10996, #17744, #19175 ) ;
#10714 = EDGE_CURVE ( 'NONE', #18181, #1305, #13040, .T. ) ;
#10715 = VERTEX_POINT ( 'NONE', #21552 ) ;
#10716 = LINE ( 'NONE', #17255, #16259 ) ;
#10717 = VERTEX_POINT ( 'NONE', #9711 ) ;
#10718 = ORIENTED_EDGE ( 'NONE', *, *, #6819, .T. ) ;
#10719 = DIRECTION ( 'NONE',  ( -1.000000000000000000, 0.000000000000000000, -0.000000000000000000 ) ) ;
#10720 = VECTOR ( 'NONE', #13641, 1000.000000000000000 ) ;
#10721 = ORIENTED_EDGE ( 'NONE', *, *, #1774, .T. ) ;
#10722 = LINE ( 'NONE', #8953, #10782 ) ;
#10723 = CYLINDRICAL_SURFACE ( 'NONE', #18451, 92.50100000000000477 ) ;
#10724 = AXIS2_PLACEMENT_3D ( 'NONE', #18304, #8021, #4695 ) ;
#10725 = FACE_OUTER_BOUND ( 'NONE', #4297, .T. ) ;
#10726 = CARTESIAN_POINT ( 'NONE',  ( -10.00000000000000888, 1.276847368961009516E-14, 103.6250000000000284 ) ) ;
#10727 = CARTESIAN_POINT ( 'NONE',  ( 10.00000000000000000, 21.69483248597444813, -16.89761061231758177 ) ) ;
#10728 = AXIS2_PLACEMENT_3D ( 'NONE', #3361, #15069, #10097 ) ;
#10729 = CARTESIAN_POINT ( 'NONE',  ( 0.000000000000000000, 61.33825423015778711, -69.23910433415882437 ) ) ;
#10730 = DIRECTION ( 'NONE',  ( 0.000000000000000000, 0.000000000000000000, 1.000000000000000000 ) ) ;
#10731 = DIRECTION ( 'NONE',  ( 1.000000000000000000, 0.000000000000000000, 0.000000000000000000 ) ) ;
#10732 = EDGE_LOOP ( 'NONE', ( #6104, #14576, #21292, #11013 ) ) ;
#10733 = CYLINDRICAL_SURFACE ( 'NONE', #14670, 3.000000000000000444 ) ;
#10734 = AXIS2_PLACEMENT_3D ( 'NONE', #17511, #16171, #2248 ) ;
#10735 = CARTESIAN_POINT ( 'NONE',  ( 0.000000000000000000, 0.000000000000000000, 0.000000000000000000 ) ) ;
#10736 = AXIS2_PLACEMENT_3D ( 'NONE', #5676, #12401, #19150 ) ;
#10737 = CARTESIAN_POINT ( 'NONE',  ( 0.000000000000000000, 27.26034713664087406, 7.182859710736605230 ) ) ;
#10738 = VERTEX_POINT ( 'NONE', #13142 ) ;
#10739 = CARTESIAN_POINT ( 'NONE',  ( 10.00000000000000000, -87.96697768756401103, -2.410567674971490604 ) ) ;
#10740 = EDGE_LOOP ( 'NONE', ( #63, #9239, #14031, #8623 ) ) ;
#10741 = AXIS2_PLACEMENT_3D ( 'NONE', #4127, #7226, #15729 ) ;
#10742 = DIRECTION ( 'NONE',  ( -1.000000000000000000, -0.000000000000000000, -0.000000000000000000 ) ) ;
#10743 = EDGE_LOOP ( 'NONE', ( #12776, #17638, #20909, #4529 ) ) ;
#10744 = ORIENTED_EDGE ( 'NONE', *, *, #6921, .F. ) ;
#10745 = DIRECTION ( 'NONE',  ( -1.000000000000000000, -0.000000000000000000, -0.000000000000000000 ) ) ;
#10746 = CIRCLE ( 'NONE', #15325, 12.00000000000000178 ) ;
#10747 = CARTESIAN_POINT ( 'NONE',  ( 0.000000000000000000, 0.000000000000000000, 0.000000000000000000 ) ) ;
#10748 = FACE_OUTER_BOUND ( 'NONE', #5304, .T. ) ;
#10749 = CARTESIAN_POINT ( 'NONE',  ( 10.00000000000000000, 60.65655256511316651, -59.63197188857461128 ) ) ;
#10750 = DIRECTION ( 'NONE',  ( 0.000000000000000000, 0.000000000000000000, 1.000000000000000000 ) ) ;
#10751 = VECTOR ( 'NONE', #14665, 1000.000000000000000 ) ;
#10752 = DIRECTION ( 'NONE',  ( -1.000000000000000000, 0.000000000000000000, 0.000000000000000000 ) ) ;
#10753 = CARTESIAN_POINT ( 'NONE',  ( 10.00000000000000000, -61.71252885873428085, 58.53847642588571887 ) ) ;
#10754 = AXIS2_PLACEMENT_3D ( 'NONE', #15918, #5764, #2445 ) ;
#10755 = VERTEX_POINT ( 'NONE', #19889 ) ;
#10756 = AXIS2_PLACEMENT_3D ( 'NONE', #7398, #14015, #2517 ) ;
#10757 = CARTESIAN_POINT ( 'NONE',  ( 0.000000000000000000, 0.000000000000000000, 0.000000000000000000 ) ) ;
#10758 = EDGE_CURVE ( 'NONE', #11402, #16302, #8571, .T. ) ;
#10759 = ORIENTED_EDGE ( 'NONE', *, *, #2457, .T. ) ;
#10760 = FACE_OUTER_BOUND ( 'NONE', #7032, .T. ) ;
#10761 = ORIENTED_EDGE ( 'NONE', *, *, #16125, .T. ) ;
#10762 = PLANE ( 'NONE',  #1402 ) ;
#10763 = AXIS2_PLACEMENT_3D ( 'NONE', #1039, #806, #2361 ) ;
#10764 = DIRECTION ( 'NONE',  ( 0.000000000000000000, 0.000000000000000000, -1.000000000000000000 ) ) ;
#10765 = AXIS2_PLACEMENT_3D ( 'NONE', #10850, #1022, #14062 ) ;
#10766 = VERTEX_POINT ( 'NONE', #21117 ) ;
#10767 = ADVANCED_FACE ( 'NONE', ( #8293 ), #3203, .F. ) ;
#10768 = AXIS2_PLACEMENT_3D ( 'NONE', #12336, #15433, #10245 ) ;
#10769 = CIRCLE ( 'NONE', #1260, 92.50100000000000477 ) ;
#10770 = ORIENTED_EDGE ( 'NONE', *, *, #144, .F. ) ;
#10771 = ORIENTED_EDGE ( 'NONE', *, *, #20124, .F. ) ;
#10772 = ORIENTED_EDGE ( 'NONE', *, *, #13560, .T. ) ;
#10773 = CARTESIAN_POINT ( 'NONE',  ( 10.00000000000000000, -80.18694381077088451, -28.37681241246736974 ) ) ;
#10774 = DIRECTION ( 'NONE',  ( -1.000000000000000000, -0.000000000000000000, 0.000000000000000000 ) ) ;
#10775 = ORIENTED_EDGE ( 'NONE', *, *, #4736, .F. ) ;
#10776 = DIRECTION ( 'NONE',  ( -1.000000000000000000, -0.000000000000000000, 0.000000000000000000 ) ) ;
#10777 = DIRECTION ( 'NONE',  ( 1.000000000000000000, 0.000000000000000000, -0.000000000000000000 ) ) ;
#10778 = DIRECTION ( 'NONE',  ( 0.000000000000000000, 8.866364432770350877E-15, -1.000000000000000000 ) ) ;
#10779 = CARTESIAN_POINT ( 'NONE',  ( 10.00000000000000000, 0.000000000000000000, 0.000000000000000000 ) ) ;
#10780 = CARTESIAN_POINT ( 'NONE',  ( 5.000000000000002665, -5.479102470011078196, 87.82926298292112222 ) ) ;
#10781 = CIRCLE ( 'NONE', #7968, 32.00000000000000000 ) ;
#10782 = VECTOR ( 'NONE', #5542, 1000.000000000000000 ) ;
#10783 = ORIENTED_EDGE ( 'NONE', *, *, #18609, .T. ) ;
#10784 = AXIS2_PLACEMENT_3D ( 'NONE', #2571, #9300, #10863 ) ;
#10785 = CARTESIAN_POINT ( 'NONE',  ( 10.00000000000000000, 0.000000000000000000, 0.000000000000000000 ) ) ;
#10786 = CIRCLE ( 'NONE', #10444, 44.99999999999999289 ) ;
#10787 = DIRECTION ( 'NONE',  ( 1.000000000000000000, 0.000000000000000000, 0.000000000000000000 ) ) ;
#10788 = EDGE_CURVE ( 'NONE', #12373, #19614, #8611, .T. ) ;
#10789 = EDGE_CURVE ( 'NONE', #11651, #2871, #12796, .T. ) ;
#10790 = DIRECTION ( 'NONE',  ( 0.000000000000000000, 0.8987940462991649282, 0.4383711467890814562 ) ) ;
#10791 = ORIENTED_EDGE ( 'NONE', *, *, #12270, .T. ) ;
#10792 = DIRECTION ( 'NONE',  ( -1.000000000000000000, 0.000000000000000000, 0.000000000000000000 ) ) ;
#10793 = ORIENTED_EDGE ( 'NONE', *, *, #14080, .T. ) ;
#10794 = CARTESIAN_POINT ( 'NONE',  ( 10.00000000000000000, -18.31866948046784316, 26.23788002993718038 ) ) ;
#10795 = ORIENTED_EDGE ( 'NONE', *, *, #4326, .F. ) ;
#10796 = ORIENTED_EDGE ( 'NONE', *, *, #15668, .F. ) ;
#10797 = AXIS2_PLACEMENT_3D ( 'NONE', #10818, #2203, #17464 ) ;
#10798 = ORIENTED_EDGE ( 'NONE', *, *, #9059, .F. ) ;
#10799 = CARTESIAN_POINT ( 'NONE',  ( 10.00000000000000000, -35.34277389771474986, -85.48288328206420772 ) ) ;
#10800 = VECTOR ( 'NONE', #1690, 1000.000000000000000 ) ;
#10801 = ORIENTED_EDGE ( 'NONE', *, *, #6624, .F. ) ;
#10802 = EDGE_CURVE ( 'NONE', #1305, #447, #19148, .T. ) ;
#10803 = CARTESIAN_POINT ( 'NONE',  ( -10.00000000000000000, 0.000000000000000000, 0.000000000000000000 ) ) ;
#10804 = CARTESIAN_POINT ( 'NONE',  ( -7.395799999999999486, 0.000000000000000000, 0.000000000000000000 ) ) ;
#10805 = LINE ( 'NONE', #3749, #5753 ) ;
#10806 = DIRECTION ( 'NONE',  ( -1.000000000000000000, 0.000000000000000000, 0.000000000000000000 ) ) ;
#10807 = EDGE_CURVE ( 'NONE', #16218, #20085, #11035, .T. ) ;
#10808 = DIRECTION ( 'NONE',  ( -1.000000000000000000, 0.000000000000000000, 0.000000000000000000 ) ) ;
#10809 = DIRECTION ( 'NONE',  ( 1.000000000000000000, 0.000000000000000000, 0.000000000000000000 ) ) ;
#10810 = CARTESIAN_POINT ( 'NONE',  ( 10.00000000000000000, 64.66851233300727131, 55.25552418572984692 ) ) ;
#10811 = FACE_OUTER_BOUND ( 'NONE', #1617, .T. ) ;
#10812 = DIRECTION ( 'NONE',  ( 0.000000000000000000, 0.5877852522924689183, 0.8090169943749504489 ) ) ;
#10813 = EDGE_CURVE ( 'NONE', #12455, #19953, #21630, .T. ) ;
#10814 = AXIS2_PLACEMENT_3D ( 'NONE', #13309, #4813, #16409 ) ;
#10815 = VECTOR ( 'NONE', #10582, 1000.000000000000000 ) ;
#10816 = EDGE_CURVE ( 'NONE', #2214, #6618, #6649, .T. ) ;
#10817 = TOROIDAL_SURFACE ( 'NONE', #6963, 114.9007999999999896, 0.2041999999999998816 ) ;
#10818 = CARTESIAN_POINT ( 'NONE',  ( -1.200000000000006617, 0.000000000000000000, 0.000000000000000000 ) ) ;
#10819 = ORIENTED_EDGE ( 'NONE', *, *, #2207, .F. ) ;
#10820 = ADVANCED_FACE ( 'NONE', ( #3428 ), #20342, .T. ) ;
#10821 = VERTEX_POINT ( 'NONE', #10269 ) ;
#10822 = ORIENTED_EDGE ( 'NONE', *, *, #13098, .T. ) ;
#10823 = VERTEX_POINT ( 'NONE', #16798 ) ;
#10824 = VERTEX_POINT ( 'NONE', #9937 ) ;
#10825 = EDGE_CURVE ( 'NONE', #1350, #19412, #19512, .T. ) ;
#10826 = DIRECTION ( 'NONE',  ( -1.000000000000000000, 0.000000000000000000, 0.000000000000000000 ) ) ;
#10827 = CIRCLE ( 'NONE', #15769, 104.9000000000000341 ) ;
#10828 = ORIENTED_EDGE ( 'NONE', *, *, #12289, .F. ) ;
#10829 = AXIS2_PLACEMENT_3D ( 'NONE', #21286, #7484, #4053 ) ;
#10830 = ADVANCED_FACE ( 'NONE', ( #21654 ), #1443, .F. ) ;
#10831 = CARTESIAN_POINT ( 'NONE',  ( -1.500000000000001332, 0.000000000000000000, 0.000000000000000000 ) ) ;
#10832 = CIRCLE ( 'NONE', #21424, 44.99999999999999289 ) ;
#10833 = DIRECTION ( 'NONE',  ( 0.000000000000000000, -1.000000000000000000, 0.000000000000000000 ) ) ;
#10834 = LINE ( 'NONE', #18918, #11127 ) ;
#10835 = DIRECTION ( 'NONE',  ( 0.000000000000000000, 0.000000000000000000, 1.000000000000000000 ) ) ;
#10836 = CYLINDRICAL_SURFACE ( 'NONE', #16470, 27.49900000000000233 ) ;
#10837 = EDGE_CURVE ( 'NONE', #215, #8987, #10329, .T. ) ;
#10838 = CARTESIAN_POINT ( 'NONE',  ( 10.00000000000000000, -2.208823992043557283, -85.03123271466938604 ) ) ;
#10839 = DIRECTION ( 'NONE',  ( 0.000000000000000000, 0.4694715627858917495, -0.8829475928589264333 ) ) ;
#10840 = CARTESIAN_POINT ( 'NONE',  ( 10.00000000000000000, 52.25832601289194201, -70.80301803122729609 ) ) ;
#10841 = ORIENTED_EDGE ( 'NONE', *, *, #14032, .F. ) ;
#10842 = DIRECTION ( 'NONE',  ( -1.000000000000000000, -0.000000000000000000, -0.000000000000000000 ) ) ;
#10843 = AXIS2_PLACEMENT_3D ( 'NONE', #5965, #12367, #21537 ) ;
#10844 = ADVANCED_FACE ( 'NONE', ( #18359 ), #8407, .F. ) ;
#10845 = VECTOR ( 'NONE', #16614, 1000.000000000000000 ) ;
#10846 = VECTOR ( 'NONE', #3406, 1000.000000000000000 ) ;
#10847 = DIRECTION ( 'NONE',  ( 0.000000000000000000, 0.2079116908177531808, 0.9781476007338069101 ) ) ;
#10848 = DIRECTION ( 'NONE',  ( 0.000000000000000000, 0.000000000000000000, 1.000000000000000000 ) ) ;
#10849 = ORIENTED_EDGE ( 'NONE', *, *, #19172, .T. ) ;
#10850 = CARTESIAN_POINT ( 'NONE',  ( 10.00000000000000000, -51.76708072107932423, 67.49339815138475274 ) ) ;
#10851 = EDGE_LOOP ( 'NONE', ( #6224, #12286, #4392, #7412 ) ) ;
#10852 = FILL_AREA_STYLE_COLOUR ( '', #6070 ) ;
#10853 = DIRECTION ( 'NONE',  ( 1.000000000000000000, 0.000000000000000000, -0.000000000000000000 ) ) ;
#10854 = ORIENTED_EDGE ( 'NONE', *, *, #20959, .T. ) ;
#10855 = VERTEX_POINT ( 'NONE', #11712 ) ;
#10856 = DIRECTION ( 'NONE',  ( -1.000000000000000000, -0.000000000000000000, -0.000000000000000000 ) ) ;
#10857 = LINE ( 'NONE', #7142, #7748 ) ;
#10858 = VECTOR ( 'NONE', #17147, 1000.000000000000000 ) ;
#10859 = TOROIDAL_SURFACE ( 'NONE', #12283, 5.633200000000004870, 0.02569999999999482421 ) ;
#10860 = CARTESIAN_POINT ( 'NONE',  ( 7.500000000000000000, 9.184850993605147944E-16, 3.000000000000000000 ) ) ;
#10861 = DIRECTION ( 'NONE',  ( -0.000000000000000000, -0.000000000000000000, 1.000000000000000000 ) ) ;
#10862 = CIRCLE ( 'NONE', #5230, 118.9000000000000199 ) ;
#10863 = DIRECTION ( 'NONE',  ( 0.000000000000000000, -0.4694715627858974671, 0.8829475928589232137 ) ) ;
#10864 = CIRCLE ( 'NONE', #1696, 11.99999999999999822 ) ;
#10865 = CARTESIAN_POINT ( 'NONE',  ( 10.00000000000000000, 36.60317927562682883, -76.78148674856727496 ) ) ;
#10866 = AXIS2_PLACEMENT_3D ( 'NONE', #3669, #12281, #19035 ) ;
#10867 = EDGE_CURVE ( 'NONE', #20371, #14005, #104, .T. ) ;
#10868 = DIRECTION ( 'NONE',  ( -1.000000000000000000, -0.000000000000000000, -0.000000000000000000 ) ) ;
#10869 = CARTESIAN_POINT ( 'NONE',  ( 10.00000000000000000, -25.56104204395359503, 81.12843256239655432 ) ) ;
#10870 = DIRECTION ( 'NONE',  ( 1.000000000000000000, 0.000000000000000000, 0.000000000000000000 ) ) ;
#10871 = ORIENTED_EDGE ( 'NONE', *, *, #13836, .F. ) ;
#10872 = DIRECTION ( 'NONE',  ( -1.000000000000000000, 0.000000000000000000, 0.000000000000000000 ) ) ;
#10873 = EDGE_LOOP ( 'NONE', ( #9619, #2322 ) ) ;
#10874 = CARTESIAN_POINT ( 'NONE',  ( 1.399999999999998579, 0.000000000000000000, 0.000000000000000000 ) ) ;
#10875 = ORIENTED_EDGE ( 'NONE', *, *, #14704, .T. ) ;
#10876 = CIRCLE ( 'NONE', #13709, 44.99999999999999289 ) ;
#10877 = FACE_OUTER_BOUND ( 'NONE', #12294, .T. ) ;
#10878 = AXIS2_PLACEMENT_3D ( 'NONE', #10032, #7862, #8393 ) ;
#10879 = AXIS2_PLACEMENT_3D ( 'NONE', #3622, #16669, #10145 ) ;
#10880 = DIRECTION ( 'NONE',  ( -1.000000000000000000, 0.000000000000000000, 0.000000000000000000 ) ) ;
#10881 = AXIS2_PLACEMENT_3D ( 'NONE', #18032, #19894, #20014 ) ;
#10882 = VERTEX_POINT ( 'NONE', #10049 ) ;
#10883 = ORIENTED_EDGE ( 'NONE', *, *, #15351, .T. ) ;
#10884 = VERTEX_POINT ( 'NONE', #5202 ) ;
#10885 = EDGE_LOOP ( 'NONE', ( #5896, #20858, #2894, #19661 ) ) ;
#10886 = CARTESIAN_POINT ( 'NONE',  ( 10.00000000000000000, 0.000000000000000000, -88.00000000000000000 ) ) ;
#10887 = DIRECTION ( 'NONE',  ( 1.000000000000000000, 0.000000000000000000, 0.000000000000000000 ) ) ;
#10888 = ORIENTED_EDGE ( 'NONE', *, *, #19752, .F. ) ;
#10889 = CARTESIAN_POINT ( 'NONE',  ( 10.00000000000000000, -46.07110168784768689, -74.97635353408431058 ) ) ;
#10890 = FACE_OUTER_BOUND ( 'NONE', #1553, .T. ) ;
#10891 = CARTESIAN_POINT ( 'NONE',  ( 10.00000000000000000, -45.60224695560514618, -80.47900393021774335 ) ) ;
#10892 = VECTOR ( 'NONE', #21279, 1000.000000000000000 ) ;
#10893 = DIRECTION ( 'NONE',  ( 0.000000000000000000, 0.2756373558169933902, 0.9612616959383204485 ) ) ;
#10894 = CARTESIAN_POINT ( 'NONE',  ( 0.000000000000000000, 87.96697768756401103, -2.410567674970879981 ) ) ;
#10895 = AXIS2_PLACEMENT_3D ( 'NONE', #9465, #2516, #16224 ) ;
#10896 = AXIS2_PLACEMENT_3D ( 'NONE', #7598, #4388, #15984 ) ;
#10897 = VECTOR ( 'NONE', #9234, 1000.000000000000000 ) ;
#10898 = ORIENTED_EDGE ( 'NONE', *, *, #19010, .F. ) ;
#10899 = CIRCLE ( 'NONE', #9130, 1.100000000000003642 ) ;
#10900 = EDGE_CURVE ( 'NONE', #1295, #19418, #8510, .T. ) ;
#10901 = DIRECTION ( 'NONE',  ( 0.000000000000000000, 0.000000000000000000, -1.000000000000000000 ) ) ;
#10902 = DIRECTION ( 'NONE',  ( -1.000000000000000000, -0.000000000000000000, -0.000000000000000000 ) ) ;
#10903 = DIRECTION ( 'NONE',  ( 0.000000000000000000, 0.000000000000000000, 1.000000000000000000 ) ) ;
#10904 = ORIENTED_EDGE ( 'NONE', *, *, #19673, .T. ) ;
#10905 = CARTESIAN_POINT ( 'NONE',  ( 10.00000000000000000, 90.63195040374188238, 18.50093422002450083 ) ) ;
#10906 = ORIENTED_EDGE ( 'NONE', *, *, #16150, .T. ) ;
#10907 = DIRECTION ( 'NONE',  ( -1.000000000000000000, 0.000000000000000000, 0.000000000000000000 ) ) ;
#10908 = EDGE_LOOP ( 'NONE', ( #16596, #17555, #4689, #11416 ) ) ;
#10909 = ORIENTED_EDGE ( 'NONE', *, *, #597, .T. ) ;
#10910 = CIRCLE ( 'NONE', #21509, 45.00000000000000000 ) ;
#10911 = ORIENTED_EDGE ( 'NONE', *, *, #992, .F. ) ;
#10912 = VECTOR ( 'NONE', #16645, 1000.000000000000114 ) ;
#10913 = DIRECTION ( 'NONE',  ( -1.000000000000000000, -0.000000000000000000, 0.000000000000000000 ) ) ;
#10914 = AXIS2_PLACEMENT_3D ( 'NONE', #14798, #9807, #6416 ) ;
#10915 = EDGE_LOOP ( 'NONE', ( #2701, #6315, #10434, #16871 ) ) ;
#10916 = CARTESIAN_POINT ( 'NONE',  ( 0.000000000000000000, 19.29292659244005392, 25.53004080487768590 ) ) ;
#10917 = LINE ( 'NONE', #3961, #16412 ) ;
#10918 = DIRECTION ( 'NONE',  ( 0.000000000000000000, 0.8660254037844363761, 0.5000000000000039968 ) ) ;
#10919 = EDGE_CURVE ( 'NONE', #2977, #20211, #469, .T. ) ;
#10920 = FACE_OUTER_BOUND ( 'NONE', #20079, .T. ) ;
#10921 = CARTESIAN_POINT ( 'NONE',  ( 9.999999999999994671, 0.000000000000000000, 0.000000000000000000 ) ) ;
#10922 = DIRECTION ( 'NONE',  ( 1.000000000000000000, 0.000000000000000000, 0.000000000000000000 ) ) ;
#10923 = LINE ( 'NONE', #18008, #3704 ) ;
#10924 = ADVANCED_FACE ( 'NONE', ( #11936 ), #3538, .F. ) ;
#10925 = LINE ( 'NONE', #20871, #14733 ) ;
#10926 = FACE_OUTER_BOUND ( 'NONE', #9541, .T. ) ;
#10927 = AXIS2_PLACEMENT_3D ( 'NONE', #7789, #16394, #1268 ) ;
#10928 = AXIS2_PLACEMENT_3D ( 'NONE', #17983, #2835, #8142 ) ;
#10929 = DIRECTION ( 'NONE',  ( 0.000000000000000000, 0.000000000000000000, 1.000000000000000000 ) ) ;
#10930 = EDGE_CURVE ( 'NONE', #11655, #11594, #10598, .T. ) ;
#10931 = EDGE_LOOP ( 'NONE', ( #19545, #767 ) ) ;
#10932 = EDGE_LOOP ( 'NONE', ( #7974, #11069, #556, #13360 ) ) ;
#10933 = EDGE_LOOP ( 'NONE', ( #9402, #6671 ) ) ;
#10934 = ORIENTED_EDGE ( 'NONE', *, *, #17805, .F. ) ;
#10935 = ORIENTED_EDGE ( 'NONE', *, *, #3887, .T. ) ;
#10936 = CYLINDRICAL_SURFACE ( 'NONE', #6659, 88.00000000000000000 ) ;
#10937 = ADVANCED_FACE ( 'NONE', ( #654 ), #10485, .F. ) ;
#10938 = VERTEX_POINT ( 'NONE', #18783 ) ;
#10939 = EDGE_CURVE ( 'NONE', #6904, #16928, #15465, .T. ) ;
#10940 = EDGE_CURVE ( 'NONE', #7162, #9877, #7501, .T. ) ;
#10941 = AXIS2_PLACEMENT_3D ( 'NONE', #11835, #11623, #16927 ) ;
#10942 = CARTESIAN_POINT ( 'NONE',  ( 10.00000000000000000, 0.000000000000000000, 0.000000000000000000 ) ) ;
#10943 = DIRECTION ( 'NONE',  ( 1.000000000000000000, 0.000000000000000000, 0.000000000000000000 ) ) ;
#10944 = EDGE_CURVE ( 'NONE', #19543, #21459, #6469, .T. ) ;
#10945 = DIRECTION ( 'NONE',  ( 0.000000000000000000, 0.3420201433256693235, -0.9396926207859080948 ) ) ;
#10946 = FACE_OUTER_BOUND ( 'NONE', #21400, .T. ) ;
#10947 = CARTESIAN_POINT ( 'NONE',  ( 10.00000000000000000, 0.000000000000000000, 0.000000000000000000 ) ) ;
#10948 = CARTESIAN_POINT ( 'NONE',  ( 10.00000000000000000, 0.000000000000000000, 0.000000000000000000 ) ) ;
#10949 = CARTESIAN_POINT ( 'NONE',  ( 5.000000000000002665, 35.18804927320642406, -80.65854690202642985 ) ) ;
#10950 = DIRECTION ( 'NONE',  ( 1.000000000000000000, 0.000000000000000000, 0.000000000000000000 ) ) ;
#10951 = ORIENTED_EDGE ( 'NONE', *, *, #7094, .F. ) ;
#10952 = CYLINDRICAL_SURFACE ( 'NONE', #17846, 88.00000000000000000 ) ;
#10953 = ADVANCED_FACE ( 'NONE', ( #13907 ), #17561, .F. ) ;
#10954 = AXIS2_PLACEMENT_3D ( 'NONE', #12374, #2321, #7712 ) ;
#10955 = CYLINDRICAL_SURFACE ( 'NONE', #21449, 88.00000000000000000 ) ;
#10956 = ADVANCED_FACE ( 'NONE', ( #17346 ), #5740, .F. ) ;
#10957 = DIRECTION ( 'NONE',  ( 0.000000000000000000, -2.698458740408367555E-15, -1.000000000000000000 ) ) ;
#10958 = EDGE_LOOP ( 'NONE', ( #2031, #12696, #7794, #4944 ) ) ;
#10959 = CYLINDRICAL_SURFACE ( 'NONE', #10765, 44.99999999999998579 ) ;
#10960 = ORIENTED_EDGE ( 'NONE', *, *, #19827, .F. ) ;
#10961 = ORIENTED_EDGE ( 'NONE', *, *, #9584, .F. ) ;
#10962 = EDGE_CURVE ( 'NONE', #18043, #9349, #2567, .T. ) ;
#10963 = SHAPE_DEFINITION_REPRESENTATION ( #9837, #10365 ) ;
#10964 = LINE ( 'NONE', #21143, #3996 ) ;
#10965 = VECTOR ( 'NONE', #4817, 1000.000000000000000 ) ;
#10966 = ORIENTED_EDGE ( 'NONE', *, *, #16658, .F. ) ;
#10967 = EDGE_LOOP ( 'NONE', ( #3825, #15957, #538, #4617 ) ) ;
#10968 = CARTESIAN_POINT ( 'NONE',  ( 10.00000000000000000, -75.45728100697627383, 39.26051685139039193 ) ) ;
#10969 = DIRECTION ( 'NONE',  ( 0.000000000000000000, 0.000000000000000000, 1.000000000000000000 ) ) ;
#10970 = EDGE_CURVE ( 'NONE', #13683, #2527, #15627, .T. ) ;
#10971 = DIRECTION ( 'NONE',  ( -1.000000000000000000, -0.000000000000000000, -0.000000000000000000 ) ) ;
#10972 = DIRECTION ( 'NONE',  ( -1.000000000000000000, 0.000000000000000000, 0.000000000000000000 ) ) ;
#10973 = DIRECTION ( 'NONE',  ( 0.000000000000000000, 0.000000000000000000, 1.000000000000000000 ) ) ;
#10974 = CIRCLE ( 'NONE', #18035, 32.00000000000000000 ) ;
#10975 = DIRECTION ( 'NONE',  ( 0.000000000000000000, -0.2756373558169869509, -0.9612616959383223358 ) ) ;
#10976 = CYLINDRICAL_SURFACE ( 'NONE', #6837, 44.99999999999999289 ) ;
#10977 = CARTESIAN_POINT ( 'NONE',  ( -1.400000000000000577, 0.000000000000000000, 0.000000000000000000 ) ) ;
#10978 = LINE ( 'NONE', #17835, #11571 ) ;
#10979 = ORIENTED_EDGE ( 'NONE', *, *, #6381, .T. ) ;
#10980 = CARTESIAN_POINT ( 'NONE',  ( 10.00000000000000000, 71.72924546249947753, 45.71766382684695884 ) ) ;
#10981 = ADVANCED_FACE ( 'NONE', ( #7293 ), #4079, .F. ) ;
#10982 = VERTEX_POINT ( 'NONE', #437 ) ;
#10983 = ADVANCED_FACE ( 'NONE', ( #8930 ), #20767, .F. ) ;
#10984 = CARTESIAN_POINT ( 'NONE',  ( 10.00000000000000000, 28.00896854772012645, -15.47571261340895532 ) ) ;
#10985 = VERTEX_POINT ( 'NONE', #19210 ) ;
#10986 =( NAMED_UNIT ( * ) SI_UNIT ( $, .STERADIAN. ) SOLID_ANGLE_UNIT ( ) );
#10987 = AXIS2_PLACEMENT_3D ( 'NONE', #3590, #18736, #15520 ) ;
#10988 = PRESENTATION_LAYER_ASSIGNMENT (  '', '', ( #2519 ) ) ;
#10989 = EDGE_CURVE ( 'NONE', #14528, #18773, #18455, .T. ) ;
#10990 = CARTESIAN_POINT ( 'NONE',  ( 10.00000000000000000, 0.000000000000000000, 0.000000000000000000 ) ) ;
#10991 = EDGE_LOOP ( 'NONE', ( #14783, #5836, #3246, #3240 ) ) ;
#10992 = ADVANCED_FACE ( 'NONE', ( #8729 ), #12142, .F. ) ;
#10993 = ORIENTED_EDGE ( 'NONE', *, *, #14464, .T. ) ;
#10994 = VERTEX_POINT ( 'NONE', #15675 ) ;
#10995 = ORIENTED_EDGE ( 'NONE', *, *, #13422, .F. ) ;
#10996 = CARTESIAN_POINT ( 'NONE',  ( 0.000000000000000000, 32.56745702629739014, 78.57830605990665163 ) ) ;
#10997 = CARTESIAN_POINT ( 'NONE',  ( 10.00000000000000000, -26.69209308833503513, -6.612652082459592684 ) ) ;
#10998 = ORIENTED_EDGE ( 'NONE', *, *, #10549, .F. ) ;
#10999 = LINE ( 'NONE', #19291, #12853 ) ;
#11000 = DIRECTION ( 'NONE',  ( 1.000000000000000000, 0.000000000000000000, 0.000000000000000000 ) ) ;
#11001 = FACE_BOUND ( 'NONE', #16075, .T. ) ;
#11002 = DIRECTION ( 'NONE',  ( 1.000000000000000000, 0.000000000000000000, 0.000000000000000000 ) ) ;
#11003 = DIRECTION ( 'NONE',  ( 1.000000000000000000, 0.000000000000000000, 0.000000000000000000 ) ) ;
#11004 = VERTEX_POINT ( 'NONE', #5634 ) ;
#11005 = CYLINDRICAL_SURFACE ( 'NONE', #9855, 44.99999999999999289 ) ;
#11006 = DIRECTION ( 'NONE',  ( -1.000000000000000000, -0.000000000000000000, 0.000000000000000000 ) ) ;
#11007 = DIRECTION ( 'NONE',  ( -0.000000000000000000, 0.000000000000000000, -1.000000000000000000 ) ) ;
#11008 = ORIENTED_EDGE ( 'NONE', *, *, #13366, .F. ) ;
#11009 = AXIS2_PLACEMENT_3D ( 'NONE', #18618, #3584, #3362 ) ;
#11010 = DIRECTION ( 'NONE',  ( -1.000000000000000000, 0.000000000000000000, 0.000000000000000000 ) ) ;
#11011 = ORIENTED_EDGE ( 'NONE', *, *, #6995, .T. ) ;
#11012 = CARTESIAN_POINT ( 'NONE',  ( 10.00000000000000000, 88.70892494636771630, -26.21376805916497332 ) ) ;
#11013 = ORIENTED_EDGE ( 'NONE', *, *, #12275, .T. ) ;
#11014 = ORIENTED_EDGE ( 'NONE', *, *, #14459, .F. ) ;
#11015 = ORIENTED_EDGE ( 'NONE', *, *, #18609, .F. ) ;
#11016 = DIRECTION ( 'NONE',  ( 1.000000000000000000, 0.000000000000000000, 0.000000000000000000 ) ) ;
#11017 = VERTEX_POINT ( 'NONE', #12363 ) ;
#11018 = DIRECTION ( 'NONE',  ( -1.000000000000000000, -0.000000000000000000, 0.000000000000000000 ) ) ;
#11019 = CIRCLE ( 'NONE', #7837, 100.0000000000000284 ) ;
#11020 = CARTESIAN_POINT ( 'NONE',  ( 5.000000000000000000, -81.34229909304657724, -33.57723005635448743 ) ) ;
#11021 = CYLINDRICAL_SURFACE ( 'NONE', #5406, 92.50100000000000477 ) ;
#11022 = DIRECTION ( 'NONE',  ( -1.000000000000000000, -0.000000000000000000, -0.000000000000000000 ) ) ;
#11023 = DIRECTION ( 'NONE',  ( 1.000000000000000000, 0.000000000000000000, -0.000000000000000000 ) ) ;
#11024 = DIRECTION ( 'NONE',  ( -1.000000000000000000, 0.000000000000000000, 0.000000000000000000 ) ) ;
#11025 = DIRECTION ( 'NONE',  ( 1.000000000000000000, 0.000000000000000000, 0.000000000000000000 ) ) ;
#11026 = AXIS2_PLACEMENT_3D ( 'NONE', #13562, #20318, #15214 ) ;
#11027 = DIRECTION ( 'NONE',  ( 0.000000000000000000, 0.000000000000000000, 1.000000000000000000 ) ) ;
#11028 = DIRECTION ( 'NONE',  ( 0.000000000000000000, 0.000000000000000000, 1.000000000000000000 ) ) ;
#11029 = DIRECTION ( 'NONE',  ( 0.000000000000000000, 0.000000000000000000, 1.000000000000000000 ) ) ;
#11030 = EDGE_LOOP ( 'NONE', ( #5818, #14772, #11941, #12075 ) ) ;
#11031 = AXIS2_PLACEMENT_3D ( 'NONE', #8928, #7173, #17345 ) ;
#11032 = EDGE_CURVE ( 'NONE', #15418, #18906, #3965, .T. ) ;
#11033 = ORIENTED_EDGE ( 'NONE', *, *, #12584, .F. ) ;
#11034 = EDGE_LOOP ( 'NONE', ( #16038, #5800, #18302, #12187 ) ) ;
#11035 = CIRCLE ( 'NONE', #18103, 88.00000000000000000 ) ;
#11036 = AXIS2_PLACEMENT_3D ( 'NONE', #20762, #18779, #5517 ) ;
#11037 = ORIENTED_EDGE ( 'NONE', *, *, #6813, .F. ) ;
#11038 = ADVANCED_FACE ( 'NONE', ( #2308 ), #9040, .T. ) ;
#11039 = CIRCLE ( 'NONE', #12441, 44.99999999999999289 ) ;
#11040 = VERTEX_POINT ( 'NONE', #1398 ) ;
#11041 = DIRECTION ( 'NONE',  ( -1.000000000000000000, -0.000000000000000000, -0.000000000000000000 ) ) ;
#11042 = VERTEX_POINT ( 'NONE', #8236 ) ;
#11043 = DIRECTION ( 'NONE',  ( 1.000000000000000000, 0.000000000000000000, 0.000000000000000000 ) ) ;
#11044 = DIRECTION ( 'NONE',  ( -1.000000000000000000, -0.000000000000000000, -0.000000000000000000 ) ) ;
#11045 = CARTESIAN_POINT ( 'NONE',  ( 10.00000000000000000, -12.90282758292962662, -25.06465718894790484 ) ) ;
#11046 = MECHANICAL_DESIGN_GEOMETRIC_PRESENTATION_REPRESENTATION (  '', ( #5421 ), #7182 ) ;
#11047 = CARTESIAN_POINT ( 'NONE',  ( 0.000000000000000000, 0.000000000000000000, 0.000000000000000000 ) ) ;
#11048 = FACE_OUTER_BOUND ( 'NONE', #2181, .T. ) ;
#11049 = DIRECTION ( 'NONE',  ( 0.000000000000000000, 0.9702957262759972501, -0.2419218955996649267 ) ) ;
#11050 = LINE ( 'NONE', #9503, #19612 ) ;
#11051 = DIRECTION ( 'NONE',  ( 0.000000000000000000, 0.000000000000000000, 1.000000000000000000 ) ) ;
#11052 = CARTESIAN_POINT ( 'NONE',  ( 10.00000000000000000, 24.73395913766480447, -12.01774797440553044 ) ) ;
#11053 = AXIS2_PLACEMENT_3D ( 'NONE', #19949, #8027, #3157 ) ;
#11054 = VERTEX_POINT ( 'NONE', #8348 ) ;
#11055 = AXIS2_PLACEMENT_3D ( 'NONE', #302, #13776, #5376 ) ;
#11056 = CARTESIAN_POINT ( 'NONE',  ( 10.00000000000000000, 27.48365448817206769, 0.9185515634842894572 ) ) ;
#11057 = VECTOR ( 'NONE', #21576, 1000.000000000000000 ) ;
#11058 = ADVANCED_FACE ( 'NONE', ( #16413 ), #14763, .F. ) ;
#11059 = ADVANCED_FACE ( 'NONE', ( #20979 ), #21092, .T. ) ;
#11060 = EDGE_CURVE ( 'NONE', #13186, #21594, #14967, .T. ) ;
#11061 = ORIENTED_EDGE ( 'NONE', *, *, #8938, .T. ) ;
#11062 = CARTESIAN_POINT ( 'NONE',  ( -90.00000000000000000, 0.000000000000000000, -104.9000000000000341 ) ) ;
#11063 = EDGE_CURVE ( 'NONE', #752, #19437, #6488, .T. ) ;
#11064 = DIRECTION ( 'NONE',  ( 0.000000000000000000, 0.000000000000000000, 1.000000000000000000 ) ) ;
#11065 = AXIS2_PLACEMENT_3D ( 'NONE', #17420, #13993, #8588 ) ;
#11066 = VERTEX_POINT ( 'NONE', #21712 ) ;
#11067 = FACE_OUTER_BOUND ( 'NONE', #14387, .T. ) ;
#11068 = ORIENTED_EDGE ( 'NONE', *, *, #3168, .F. ) ;
#11069 = ORIENTED_EDGE ( 'NONE', *, *, #11342, .F. ) ;
#11070 = APPLICATION_PROTOCOL_DEFINITION ( 'draft international standard', 'automotive_design', 1998, #7281 ) ;
#11071 = AXIS2_PLACEMENT_3D ( 'NONE', #15945, #4017, #14286 ) ;
#11072 = DIRECTION ( 'NONE',  ( 0.000000000000000000, 0.4067366430757948237, 0.9135454576426033091 ) ) ;
#11073 = VERTEX_POINT ( 'NONE', #15997 ) ;
#11074 = ORIENTED_EDGE ( 'NONE', *, *, #18284, .F. ) ;
#11075 = DIRECTION ( 'NONE',  ( -1.000000000000000000, 0.000000000000000000, 0.000000000000000000 ) ) ;
#11076 = AXIS2_PLACEMENT_3D ( 'NONE', #5600, #17315, #2379 ) ;
#11077 = DIRECTION ( 'NONE',  ( -1.000000000000000000, 0.000000000000000000, 0.000000000000000000 ) ) ;
#11078 = EDGE_CURVE ( 'NONE', #17938, #2662, #8242, .T. ) ;
#11079 = DIRECTION ( 'NONE',  ( -1.000000000000000000, -0.000000000000000000, 0.000000000000000000 ) ) ;
#11080 = FACE_OUTER_BOUND ( 'NONE', #2256, .T. ) ;
#11081 = CARTESIAN_POINT ( 'NONE',  ( -10.00000000000000888, 0.000000000000000000, 0.000000000000000000 ) ) ;
#11082 = DIRECTION ( 'NONE',  ( 0.000000000000000000, -0.4067366430757887175, -0.9135454576426059736 ) ) ;
#11083 = DIRECTION ( 'NONE',  ( 0.000000000000000000, 0.000000000000000000, 1.000000000000000000 ) ) ;
#11084 = ADVANCED_FACE ( 'NONE', ( #13196 ), #6596, .T. ) ;
#11085 = DIRECTION ( 'NONE',  ( 1.000000000000000000, -0.000000000000000000, 0.000000000000000000 ) ) ;
#11086 = DIRECTION ( 'NONE',  ( 1.000000000000000000, -0.000000000000000000, -0.000000000000000000 ) ) ;
#11087 = AXIS2_PLACEMENT_3D ( 'NONE', #10865, #14173, #20920 ) ;
#11088 = ORIENTED_EDGE ( 'NONE', *, *, #4847, .T. ) ;
#11089 = DIRECTION ( 'NONE',  ( 0.000000000000000000, 0.9945218953682737340, -0.1045284632676505010 ) ) ;
#11090 = VECTOR ( 'NONE', #20421, 1000.000000000000000 ) ;
#11091 = ORIENTED_EDGE ( 'NONE', *, *, #10867, .F. ) ;
#11092 = EDGE_CURVE ( 'NONE', #20880, #21758, #117, .T. ) ;
#11093 = VECTOR ( 'NONE', #2032, 1000.000000000000000 ) ;
#11094 = DIRECTION ( 'NONE',  ( 1.000000000000000000, 0.000000000000000000, 0.000000000000000000 ) ) ;
#11095 = ADVANCED_FACE ( 'NONE', ( #16528 ), #19833, .F. ) ;
#11096 = PRESENTATION_STYLE_ASSIGNMENT (( #17958 ) ) ;
#11097 = CYLINDRICAL_SURFACE ( 'NONE', #19386, 104.9000000000000341 ) ;
#11098 = EDGE_LOOP ( 'NONE', ( #11676, #3848, #76, #4857 ) ) ;
#11099 = AXIS2_PLACEMENT_3D ( 'NONE', #14513, #21253, #19055 ) ;
#11100 = VERTEX_POINT ( 'NONE', #14868 ) ;
#11101 = ORIENTED_EDGE ( 'NONE', *, *, #13658, .T. ) ;
#11102 = CIRCLE ( 'NONE', #20632, 11.99999999999999645 ) ;
#11103 = ORIENTED_EDGE ( 'NONE', *, *, #15907, .F. ) ;
#11104 = DIRECTION ( 'NONE',  ( 1.000000000000000000, 0.000000000000000000, 0.000000000000000000 ) ) ;
#11105 = CARTESIAN_POINT ( 'NONE',  ( -90.00000000000000000, 0.000000000000000000, -5.612499999999999822 ) ) ;
#11106 = ORIENTED_EDGE ( 'NONE', *, *, #5159, .F. ) ;
#11107 = VECTOR ( 'NONE', #4395, 1000.000000000000000 ) ;
#11108 = EDGE_CURVE ( 'NONE', #5155, #20330, #1287, .T. ) ;
#11109 = CIRCLE ( 'NONE', #21689, 11.99999999999999822 ) ;
#11110 = DIRECTION ( 'NONE',  ( 1.000000000000000000, 0.000000000000000000, 0.000000000000000000 ) ) ;
#11111 = CARTESIAN_POINT ( 'NONE',  ( 10.00000000000000000, 67.05625154133539922, -63.71729851637743280 ) ) ;
#11112 = CARTESIAN_POINT ( 'NONE',  ( 10.00000000000000000, -84.79630770241078608, -6.691460262316255125 ) ) ;
#11113 = EDGE_CURVE ( 'NONE', #12476, #18185, #17772, .T. ) ;
#11114 = DIRECTION ( 'NONE',  ( 0.000000000000000000, 0.06975647374411841906, 0.9975640502598247528 ) ) ;
#11115 = CIRCLE ( 'NONE', #16761, 113.8250000000000028 ) ;
#11116 = DIRECTION ( 'NONE',  ( 0.000000000000000000, -9.251858538542973800E-16, -1.000000000000000000 ) ) ;
#11117 = ADVANCED_FACE ( 'NONE', ( #4816 ), #20588, .T. ) ;
#11118 = EDGE_LOOP ( 'NONE', ( #3529, #12354, #13744, #10095 ) ) ;
#11119 = EDGE_CURVE ( 'NONE', #17876, #20049, #1535, .T. ) ;
#11120 = CARTESIAN_POINT ( 'NONE',  ( 10.00000000000000000, 6.797690662955227836, 87.73705831432218361 ) ) ;
#11121 = DIRECTION ( 'NONE',  ( -1.000000000000000000, -0.000000000000000000, -0.000000000000000000 ) ) ;
#11122 = ORIENTED_EDGE ( 'NONE', *, *, #9889, .F. ) ;
#11123 = AXIS2_PLACEMENT_3D ( 'NONE', #7274, #3734, #5391 ) ;
#11124 = VECTOR ( 'NONE', #16513, 1000.000000000000000 ) ;
#11125 = CIRCLE ( 'NONE', #878, 11.99999999999999822 ) ;
#11126 = CARTESIAN_POINT ( 'NONE',  ( 9.999999999999994671, 1.269040245616444393E-14, -103.6249999999999716 ) ) ;
#11127 = VECTOR ( 'NONE', #3775, 1000.000000000000000 ) ;
#11128 = ORIENTED_EDGE ( 'NONE', *, *, #3390, .T. ) ;
#11129 = EDGE_CURVE ( 'NONE', #19437, #7036, #13314, .T. ) ;
#11130 = FACE_BOUND ( 'NONE', #10632, .T. ) ;
#11131 = DIRECTION ( 'NONE',  ( -1.000000000000000000, -0.000000000000000000, -0.000000000000000000 ) ) ;
#11132 = ORIENTED_EDGE ( 'NONE', *, *, #1722, .F. ) ;
#11133 = CARTESIAN_POINT ( 'NONE',  ( 0.000000000000000000, -31.88200538760795766, 2.745493118646878727 ) ) ;
#11134 = EDGE_LOOP ( 'NONE', ( #12698, #11630, #17145, #17359 ) ) ;
#11135 = EDGE_LOOP ( 'NONE', ( #18828, #1278, #6560, #14028 ) ) ;
#11136 = ORIENTED_EDGE ( 'NONE', *, *, #1249, .T. ) ;
#11137 = CLOSED_SHELL ( 'NONE', ( #11117, #20841, #3233, #18257, #12338, #19449, #16857, #8517, #20549, #9752, #16370, #4686, #4114, #694, #4863, #8520, #2284, #20173, #3146, #17436, #9208, #18795, #16631, #21207, #9140, #19623, #9966, #15623, #13620, #9216, #1142, #7479, #1762, #17839, #13397, #6818, #985, #8542, #1001, #5815, #8887, #20439, #10370, #5683 ) ) ;
#11138 = LINE ( 'NONE', #21731, #13583 ) ;
#11139 = ORIENTED_EDGE ( 'NONE', *, *, #9437, .F. ) ;
#11140 = DIRECTION ( 'NONE',  ( -1.000000000000000000, -0.000000000000000000, 0.000000000000000000 ) ) ;
#11141 = FACE_OUTER_BOUND ( 'NONE', #2912, .T. ) ;
#11142 = CYLINDRICAL_SURFACE ( 'NONE', #3292, 32.00000000000000000 ) ;
#11143 = AXIS2_PLACEMENT_3D ( 'NONE', #9721, #14379, #21133 ) ;
#11144 = VECTOR ( 'NONE', #7128, 1000.000000000000000 ) ;
#11145 = AXIS2_PLACEMENT_3D ( 'NONE', #3587, #20496, #6916 ) ;
#11146 = CARTESIAN_POINT ( 'NONE',  ( 10.00000000000000000, -36.60317927562628881, 76.78148674856751654 ) ) ;
#11147 = FACE_OUTER_BOUND ( 'NONE', #19503, .T. ) ;
#11148 = DIRECTION ( 'NONE',  ( 0.000000000000000000, 0.5877852522924742473, -0.8090169943749465631 ) ) ;
#11149 = FACE_BOUND ( 'NONE', #16718, .T. ) ;
#11150 = DIRECTION ( 'NONE',  ( 1.000000000000000000, 0.000000000000000000, 0.000000000000000000 ) ) ;
#11151 = ORIENTED_EDGE ( 'NONE', *, *, #19607, .F. ) ;
#11152 = ORIENTED_EDGE ( 'NONE', *, *, #6089, .T. ) ;
#11153 = AXIS2_PLACEMENT_3D ( 'NONE', #16169, #21792, #6683 ) ;
#11154 = EDGE_LOOP ( 'NONE', ( #3087, #19682, #12836, #3948 ) ) ;
#11155 = AXIS2_PLACEMENT_3D ( 'NONE', #1743, #11044, #17795 ) ;
#11156 = ORIENTED_EDGE ( 'NONE', *, *, #254, .F. ) ;
#11157 = ORIENTED_EDGE ( 'NONE', *, *, #18689, .F. ) ;
#11158 = DIRECTION ( 'NONE',  ( 1.000000000000000000, 0.000000000000000000, 0.000000000000000000 ) ) ;
#11159 = VERTEX_POINT ( 'NONE', #9775 ) ;
#11160 = DIRECTION ( 'NONE',  ( 0.000000000000000000, 1.000000000000000000, 0.000000000000000000 ) ) ;
#11162 = EDGE_CURVE ( 'NONE', #10498, #10717, #10347, .T. ) ;
#11161 = CARTESIAN_POINT ( 'NONE',  ( 0.000000000000000000, 0.000000000000000000, 0.000000000000000000 ) ) ;
#11163 = CARTESIAN_POINT ( 'NONE',  ( 0.000000000000000000, -84.12297548659712731, -12.59025161327086906 ) ) ;
#11164 = DIRECTION ( 'NONE',  ( 0.000000000000000000, 0.000000000000000000, 1.000000000000000000 ) ) ;
#11165 = EDGE_CURVE ( 'NONE', #14878, #14805, #19426, .T. ) ;
#11166 = CIRCLE ( 'NONE', #13645, 11.99999999999999822 ) ;
#11167 = CARTESIAN_POINT ( 'NONE',  ( 0.000000000000000000, 80.18694381077148137, -28.37681241246572483 ) ) ;
#11168 = CIRCLE ( 'NONE', #7300, 11.99999999999999822 ) ;
#11169 = DIRECTION ( 'NONE',  ( -1.000000000000000000, -0.000000000000000000, -0.000000000000000000 ) ) ;
#11170 = DIRECTION ( 'NONE',  ( 0.000000000000000000, 0.000000000000000000, 1.000000000000000000 ) ) ;
#11171 = DIRECTION ( 'NONE',  ( -1.000000000000000000, -0.000000000000000000, -0.000000000000000000 ) ) ;
#11172 = ORIENTED_EDGE ( 'NONE', *, *, #15303, .F. ) ;
#11173 = PRODUCT_RELATED_PRODUCT_CATEGORY ( 'part', '', ( #4726 ) ) ;
#11174 = CARTESIAN_POINT ( 'NONE',  ( -10.00000000000000000, 0.000000000000000000, 0.000000000000000000 ) ) ;
#11175 = EDGE_LOOP ( 'NONE', ( #14929, #3492, #21289, #12586 ) ) ;
#11176 = CARTESIAN_POINT ( 'NONE',  ( -10.00000000000001954, 113.8250000000000028, 0.000000000000000000 ) ) ;
#11177 = VECTOR ( 'NONE', #3640, 1000.000000000000000 ) ;
#11178 = FACE_OUTER_BOUND ( 'NONE', #10306, .T. ) ;
#11179 = ORIENTED_EDGE ( 'NONE', *, *, #17493, .F. ) ;
#11180 = AXIS2_PLACEMENT_3D ( 'NONE', #19091, #20749, #6958 ) ;
#11181 = CARTESIAN_POINT ( 'NONE',  ( 0.000000000000000000, 0.000000000000000000, 0.000000000000000000 ) ) ;
#11182 = VERTEX_POINT ( 'NONE', #11559 ) ;
#11183 = VERTEX_POINT ( 'NONE', #1493 ) ;
#11184 = AXIS2_PLACEMENT_3D ( 'NONE', #6758, #10050, #20223 ) ;
#11185 = LINE ( 'NONE', #17935, #3648 ) ;
#11186 = EDGE_LOOP ( 'NONE', ( #6722, #17502, #10961, #7440 ) ) ;
#11187 = ORIENTED_EDGE ( 'NONE', *, *, #4363, .T. ) ;
#11188 = DIRECTION ( 'NONE',  ( 0.000000000000000000, 0.7431448254773953543, -0.6691306063588570163 ) ) ;
#11189 = DIRECTION ( 'NONE',  ( 0.000000000000000000, 0.000000000000000000, 1.000000000000000000 ) ) ;
#11190 = DIRECTION ( 'NONE',  ( 0.000000000000000000, 0.000000000000000000, 1.000000000000000000 ) ) ;
#11191 = CARTESIAN_POINT ( 'NONE',  ( 0.000000000000000000, 0.000000000000000000, -3.000000000000000000 ) ) ;
#11192 = EDGE_CURVE ( 'NONE', #5435, #7874, #12203, .T. ) ;
#11193 = DIRECTION ( 'NONE',  ( 0.000000000000000000, 1.224646799147355426E-16, 1.000000000000000000 ) ) ;
#11194 = CARTESIAN_POINT ( 'NONE',  ( 0.000000000000000000, 0.000000000000000000, 0.000000000000000000 ) ) ;
#11195 = DIRECTION ( 'NONE',  ( -1.000000000000000000, 0.000000000000000000, 0.000000000000000000 ) ) ;
#11196 = DIRECTION ( 'NONE',  ( 0.000000000000000000, 0.000000000000000000, -1.000000000000000000 ) ) ;
#11197 = CARTESIAN_POINT ( 'NONE',  ( 10.00000000000000000, 28.15804365424195765, 1.358152127006451826 ) ) ;
#11198 = CIRCLE ( 'NONE', #1676, 27.49900000000000233 ) ;
#11199 = CIRCLE ( 'NONE', #20732, 44.99999999999999289 ) ;
#11200 = ORIENTED_EDGE ( 'NONE', *, *, #811, .T. ) ;
#11201 = VECTOR ( 'NONE', #10248, 1000.000000000000000 ) ;
#11202 = AXIS2_PLACEMENT_3D ( 'NONE', #18077, #2932, #7585 ) ;
#11203 = LINE ( 'NONE', #14518, #21028 ) ;
#11204 = ORIENTED_EDGE ( 'NONE', *, *, #15040, .T. ) ;
#11205 = DIRECTION ( 'NONE',  ( 0.000000000000000000, 0.000000000000000000, -1.000000000000000000 ) ) ;
#11206 = ADVANCED_FACE ( 'NONE', ( #11877 ), #20600, .F. ) ;
#11207 = DIRECTION ( 'NONE',  ( 0.000000000000000000, 0.000000000000000000, 1.000000000000000000 ) ) ;
#11208 = EDGE_LOOP ( 'NONE', ( #21080, #16194, #1867, #3596 ) ) ;
#11209 = EDGE_CURVE ( 'NONE', #4988, #21757, #8563, .T. ) ;
#11210 = CIRCLE ( 'NONE', #1694, 92.50100000000000477 ) ;
#11211 = VERTEX_POINT ( 'NONE', #15189 ) ;
#11212 = ORIENTED_EDGE ( 'NONE', *, *, #14581, .T. ) ;
#11213 = CIRCLE ( 'NONE', #19337, 88.00000000000000000 ) ;
#11214 = ORIENTED_EDGE ( 'NONE', *, *, #2553, .F. ) ;
#11215 = AXIS2_PLACEMENT_3D ( 'NONE', #19080, #18863, #2169 ) ;
#11216 = CARTESIAN_POINT ( 'NONE',  ( 5.000000000000000000, 8.660254037844385522, 15.00000000000000000 ) ) ;
#11217 = LINE ( 'NONE', #16192, #1342 ) ;
#11218 = VECTOR ( 'NONE', #16502, 1000.000000000000000 ) ;
#11219 = ORIENTED_EDGE ( 'NONE', *, *, #2386, .T. ) ;
#11220 = EDGE_CURVE ( 'NONE', #7792, #142, #10694, .T. ) ;
#11221 = DIRECTION ( 'NONE',  ( 1.000000000000000000, 0.000000000000000000, 0.000000000000000000 ) ) ;
#11222 = CARTESIAN_POINT ( 'NONE',  ( 10.00000000000000000, 79.66702613806774025, -29.80527447819464371 ) ) ;
#11223 = ADVANCED_FACE ( 'NONE', ( #13427 ), #15291, .F. ) ;
#11224 = DIRECTION ( 'NONE',  ( -1.000000000000000000, 0.000000000000000000, 0.000000000000000000 ) ) ;
#11225 = EDGE_CURVE ( 'NONE', #1128, #3829, #9997, .T. ) ;
#11226 = CARTESIAN_POINT ( 'NONE',  ( 1.500000000000001332, 0.000000000000000000, 0.000000000000000000 ) ) ;
#11227 = DIRECTION ( 'NONE',  ( 1.000000000000000000, 0.000000000000000000, 0.000000000000000000 ) ) ;
#11228 = EDGE_CURVE ( 'NONE', #18352, #1974, #20499, .T. ) ;
#11229 = ORIENTED_EDGE ( 'NONE', *, *, #18439, .T. ) ;
#11230 = DIRECTION ( 'NONE',  ( 0.000000000000000000, 0.000000000000000000, 1.000000000000000000 ) ) ;
#11231 = DIRECTION ( 'NONE',  ( -1.000000000000000000, -0.000000000000000000, -0.000000000000000000 ) ) ;
#11232 = VERTEX_POINT ( 'NONE', #18947 ) ;
#11233 = AXIS2_PLACEMENT_3D ( 'NONE', #6225, #12941, #20355 ) ;
#11234 = AXIS2_PLACEMENT_3D ( 'NONE', #19562, #7527, #4219 ) ;
#11235 = DIRECTION ( 'NONE',  ( 0.000000000000000000, 0.000000000000000000, 1.000000000000000000 ) ) ;
#11236 = EDGE_CURVE ( 'NONE', #3628, #8974, #2937, .T. ) ;
#11237 = ORIENTED_EDGE ( 'NONE', *, *, #7628, .T. ) ;
#11238 = FACE_OUTER_BOUND ( 'NONE', #615, .T. ) ;
#11239 = DIRECTION ( 'NONE',  ( -1.000000000000000000, 0.000000000000000000, -0.000000000000000000 ) ) ;
#11240 = ORIENTED_EDGE ( 'NONE', *, *, #5305, .F. ) ;
#11241 = CARTESIAN_POINT ( 'NONE',  ( 10.00000000000000000, 76.53853822673980289, 43.42639941457142072 ) ) ;
#11242 = ADVANCED_FACE ( 'NONE', ( #20395 ), #10320, .F. ) ;
#11243 = ORIENTED_EDGE ( 'NONE', *, *, #14459, .T. ) ;
#11244 = ORIENTED_EDGE ( 'NONE', *, *, #19774, .T. ) ;
#11245 = DIRECTION ( 'NONE',  ( 0.000000000000000000, -0.9993908270190954291, -0.03489949670251119018 ) ) ;
#11246 = EDGE_CURVE ( 'NONE', #2625, #971, #16967, .T. ) ;
#11247 = ORIENTED_EDGE ( 'NONE', *, *, #4325, .T. ) ;
#11248 = DIRECTION ( 'NONE',  ( -1.000000000000000000, 0.000000000000000000, -0.000000000000000000 ) ) ;
#11249 = AXIS2_PLACEMENT_3D ( 'NONE', #1657, #15021, #3309 ) ;
#11250 = CARTESIAN_POINT ( 'NONE',  ( 10.00000000000000000, -89.12061559554348378, 24.77803214283513356 ) ) ;
#11251 = DIRECTION ( 'NONE',  ( 0.000000000000000000, 0.000000000000000000, -1.000000000000000000 ) ) ;
#11252 = AXIS2_PLACEMENT_3D ( 'NONE', #12671, #16099, #4174 ) ;
#11253 = AXIS2_PLACEMENT_3D ( 'NONE', #21073, #2086, #18989 ) ;
#11254 = AXIS2_PLACEMENT_3D ( 'NONE', #9921, #16663, #12789 ) ;
#11255 = EDGE_CURVE ( 'NONE', #16595, #18563, #6119, .T. ) ;
#11256 = DIRECTION ( 'NONE',  ( 0.000000000000000000, 0.000000000000000000, 1.000000000000000000 ) ) ;
#11257 = CARTESIAN_POINT ( 'NONE',  ( 10.00000000000000000, -85.54350296776095774, -20.64725405482940346 ) ) ;
#11259 = EDGE_CURVE ( 'NONE', #5395, #1178, #13642, .T. ) ;
#11258 = DIRECTION ( 'NONE',  ( -1.000000000000000000, 0.000000000000000000, 0.000000000000000000 ) ) ;
#11260 = DIRECTION ( 'NONE',  ( -1.000000000000000000, 0.000000000000000000, -0.000000000000000000 ) ) ;
#11261 = CARTESIAN_POINT ( 'NONE',  ( 0.000000000000000000, 32.56745702629844175, -78.57830605990621109 ) ) ;
#11262 = CIRCLE ( 'NONE', #20090, 44.99999999999998579 ) ;
#11263 = ORIENTED_EDGE ( 'NONE', *, *, #18830, .T. ) ;
#11264 = AXIS2_PLACEMENT_3D ( 'NONE', #13769, #3707, #15530 ) ;
#11265 = VERTEX_POINT ( 'NONE', #10541 ) ;
#11266 = VECTOR ( 'NONE', #6608, 1000.000000000000000 ) ;
#11267 = EDGE_CURVE ( 'NONE', #21645, #3268, #17070, .T. ) ;
#11268 = CIRCLE ( 'NONE', #21512, 11.99999999999999822 ) ;
#11269 = ORIENTED_EDGE ( 'NONE', *, *, #9480, .F. ) ;
#11270 = ORIENTED_EDGE ( 'NONE', *, *, #12312, .F. ) ;
#11271 = EDGE_CURVE ( 'NONE', #19516, #21566, #14938, .T. ) ;
#11272 = VERTEX_POINT ( 'NONE', #279 ) ;
#11273 = DIRECTION ( 'NONE',  ( 0.000000000000000000, 0.000000000000000000, 1.000000000000000000 ) ) ;
#11274 = VERTEX_POINT ( 'NONE', #1720 ) ;
#11275 = LINE ( 'NONE', #14580, #7842 ) ;
#11276 = DIRECTION ( 'NONE',  ( -1.000000000000000000, 0.000000000000000000, 0.000000000000000000 ) ) ;
#11277 = AXIS2_PLACEMENT_3D ( 'NONE', #16939, #4783, #8317 ) ;
#11278 = CYLINDRICAL_SURFACE ( 'NONE', #19249, 92.50100000000000477 ) ;
#11279 = CARTESIAN_POINT ( 'NONE',  ( 10.00000000000000000, 85.54350296776139828, -20.64725405482768750 ) ) ;
#11280 = DIRECTION ( 'NONE',  ( -1.000000000000000000, -0.000000000000000000, -0.000000000000000000 ) ) ;
#11281 = AXIS2_PLACEMENT_3D ( 'NONE', #3030, #21804, #1585 ) ;
#11282 = AXIS2_PLACEMENT_3D ( 'NONE', #18312, #1293, #4823 ) ;
#11283 = CARTESIAN_POINT ( 'NONE',  ( 10.00000000000000000, 0.000000000000000000, 0.000000000000000000 ) ) ;
#11284 = CYLINDRICAL_SURFACE ( 'NONE', #10881, 92.50100000000000477 ) ;
#11285 = ORIENTED_EDGE ( 'NONE', *, *, #14894, .F. ) ;
#11286 = LINE ( 'NONE', #9391, #3379 ) ;
#11287 = ORIENTED_EDGE ( 'NONE', *, *, #20175, .F. ) ;
#11288 = DIRECTION ( 'NONE',  ( 0.000000000000000000, 1.224646799147353207E-16, 1.000000000000000000 ) ) ;
#11289 = DIRECTION ( 'NONE',  ( 0.000000000000000000, -0.9702957262759988044, 0.2419218955996582376 ) ) ;
#11290 = ORIENTED_EDGE ( 'NONE', *, *, #5316, .F. ) ;
#11291 = AXIS2_PLACEMENT_3D ( 'NONE', #6441, #20022, #3215 ) ;
#11292 = DIRECTION ( 'NONE',  ( 1.000000000000000000, 0.000000000000000000, 0.000000000000000000 ) ) ;
#11293 = VERTEX_POINT ( 'NONE', #10431 ) ;
#11294 = EDGE_LOOP ( 'NONE', ( #5194, #18631 ) ) ;
#11295 = DIRECTION ( 'NONE',  ( 0.2281086410251079444, 0.000000000000000000, -0.9736356854027479191 ) ) ;
#11296 = CARTESIAN_POINT ( 'NONE',  ( 10.00000000000000000, 27.07404830566976983, -4.815694066514164540 ) ) ;
#11297 = ORIENTED_EDGE ( 'NONE', *, *, #6637, .F. ) ;
#11298 = ORIENTED_EDGE ( 'NONE', *, *, #14032, .T. ) ;
#11299 = CARTESIAN_POINT ( 'NONE',  ( 8.899999999999991473, 0.000000000000000000, 0.000000000000000000 ) ) ;
#11300 = CARTESIAN_POINT ( 'NONE',  ( 10.00000000000000000, 17.70753755129037188, 21.03896658273978559 ) ) ;
#11301 = CYLINDRICAL_SURFACE ( 'NONE', #20635, 44.99999999999999289 ) ;
#11302 = DIRECTION ( 'NONE',  ( 0.000000000000000000, 0.000000000000000000, -1.000000000000000000 ) ) ;
#11303 = CARTESIAN_POINT ( 'NONE',  ( 10.00000000000000000, 23.10190250628834718, 89.56973317806607326 ) ) ;
#11304 = CARTESIAN_POINT ( 'NONE',  ( 10.00000000000000000, 43.18649929580291058, -73.28107340219372645 ) ) ;
#11305 = DIRECTION ( 'NONE',  ( 0.000000000000000000, 0.000000000000000000, 1.000000000000000000 ) ) ;
#11306 = CARTESIAN_POINT ( 'NONE',  ( 0.000000000000000000, -79.38136668499764426, 37.98155635597287016 ) ) ;
#11307 = FACE_OUTER_BOUND ( 'NONE', #4397, .T. ) ;
#11308 = VECTOR ( 'NONE', #16430, 1000.000000000000000 ) ;
#11309 = ORIENTED_EDGE ( 'NONE', *, *, #56, .T. ) ;
#11310 = ORIENTED_EDGE ( 'NONE', *, *, #10008, .F. ) ;
#11311 = CARTESIAN_POINT ( 'NONE',  ( 0.000000000000000000, 85.54350296776139828, -20.64725405482768750 ) ) ;
#11312 = EDGE_CURVE ( 'NONE', #4606, #13627, #20171, .T. ) ;
#11313 = DIRECTION ( 'NONE',  ( 0.000000000000000000, -0.5877852522924797984, 0.8090169943749426773 ) ) ;
#11314 = VERTEX_POINT ( 'NONE', #2043 ) ;
#11315 = ORIENTED_EDGE ( 'NONE', *, *, #17703, .F. ) ;
#11316 = ORIENTED_EDGE ( 'NONE', *, *, #8527, .F. ) ;
#11317 = ORIENTED_EDGE ( 'NONE', *, *, #11624, .T. ) ;
#11318 =( GEOMETRIC_REPRESENTATION_CONTEXT ( 3 ) GLOBAL_UNCERTAINTY_ASSIGNED_CONTEXT ( ( #14969 ) ) GLOBAL_UNIT_ASSIGNED_CONTEXT ( ( #17738, #16286, #18179 ) ) REPRESENTATION_CONTEXT ( 'NONE', 'WORKASPACE' ) );
#11319 = DIRECTION ( 'NONE',  ( 1.000000000000000000, 0.000000000000000000, 0.000000000000000000 ) ) ;
#11320 = CARTESIAN_POINT ( 'NONE',  ( 10.00000000000000000, 62.44821182181090791, 68.23969402963524544 ) ) ;
#11321 = ADVANCED_FACE ( 'NONE', ( #5030 ), #11767, .F. ) ;
#11322 = ORIENTED_EDGE ( 'NONE', *, *, #6379, .T. ) ;
#11323 = LINE ( 'NONE', #6265, #5091 ) ;
#11324 = LINE ( 'NONE', #1488, #20408 ) ;
#11325 = CARTESIAN_POINT ( 'NONE',  ( -1.500346250137462226E-14, 60.00000000000001421, 0.000000000000000000 ) ) ;
#11326 = CYLINDRICAL_SURFACE ( 'NONE', #16713, 44.99999999999998579 ) ;
#11327 = CARTESIAN_POINT ( 'NONE',  ( 10.00000000000000000, 27.26034713664097353, 4.817140289263753594 ) ) ;
#11328 = EDGE_CURVE ( 'NONE', #6130, #13441, #3306, .T. ) ;
#11329 = ORIENTED_EDGE ( 'NONE', *, *, #13691, .T. ) ;
#11330 = CARTESIAN_POINT ( 'NONE',  ( 5.000000000000000000, 36.39558101400138668, 80.12091913260394449 ) ) ;
#11331 = CARTESIAN_POINT ( 'NONE',  ( 0.000000000000000000, 15.32665449652044565, -91.22241316115403720 ) ) ;
#11332 = ORIENTED_EDGE ( 'NONE', *, *, #16943, .T. ) ;
#11333 = PRESENTATION_LAYER_ASSIGNMENT (  '', '', ( #20866 ) ) ;
#11334 = CARTESIAN_POINT ( 'NONE',  ( 10.00000000000000000, 82.02147376274727719, -42.76579056660780509 ) ) ;
#11335 = ORIENTED_EDGE ( 'NONE', *, *, #3102, .T. ) ;
#11336 = CARTESIAN_POINT ( 'NONE',  ( 10.00000000000000888, 0.000000000000000000, 0.000000000000000000 ) ) ;
#11337 = ADVANCED_FACE ( 'NONE', ( #17512 ), #9302, .F. ) ;
#11338 = EDGE_CURVE ( 'NONE', #11363, #3657, #14572, .T. ) ;
#11339 = DIRECTION ( 'NONE',  ( 1.000000000000000000, 0.000000000000000000, 0.000000000000000000 ) ) ;
#11340 = ORIENTED_EDGE ( 'NONE', *, *, #5560, .F. ) ;
#11341 = LINE ( 'NONE', #12893, #11308 ) ;
#11342 = EDGE_CURVE ( 'NONE', #1609, #17412, #20231, .T. ) ;
#11343 = VERTEX_POINT ( 'NONE', #7666 ) ;
#11344 = ORIENTED_EDGE ( 'NONE', *, *, #13953, .T. ) ;
#11345 = CARTESIAN_POINT ( 'NONE',  ( 0.000000000000000000, 0.000000000000000000, 0.000000000000000000 ) ) ;
#11346 = ORIENTED_EDGE ( 'NONE', *, *, #17320, .F. ) ;
#11347 = FACE_OUTER_BOUND ( 'NONE', #14954, .T. ) ;
#11348 = CARTESIAN_POINT ( 'NONE',  ( 10.00000000000000000, -27.00677879429080974, 80.65868421664423238 ) ) ;
#11349 = CARTESIAN_POINT ( 'NONE',  ( -5.000000000000000000, 70.00000000000000000, 15.00000000000000000 ) ) ;
#11350 = AXIS2_PLACEMENT_3D ( 'NONE', #3939, #17421, #2276 ) ;
#11351 = DIRECTION ( 'NONE',  ( -1.000000000000000000, 0.000000000000000000, 0.000000000000000000 ) ) ;
#11352 = ADVANCED_FACE ( 'NONE', ( #805 ), #10976, .F. ) ;
#11353 = CYLINDRICAL_SURFACE ( 'NONE', #21079, 100.0000000000000000 ) ;
#11354 = DIRECTION ( 'NONE',  ( 0.000000000000000000, -0.8290375725550467312, 0.5591929034707392443 ) ) ;
#11356 = CIRCLE ( 'NONE', #15232, 27.49900000000000233 ) ;
#11355 = DIRECTION ( 'NONE',  ( 0.000000000000000000, 3.546545773108139720E-14, -1.000000000000000000 ) ) ;
#11357 = ADVANCED_FACE ( 'NONE', ( #21036 ), #7552, .T. ) ;
#11358 = AXIS2_PLACEMENT_3D ( 'NONE', #2659, #4218, #20797 ) ;
#11359 = CARTESIAN_POINT ( 'NONE',  ( 10.00000000000000000, -24.17932380791704716, -20.96092317127029503 ) ) ;
#11360 = DIRECTION ( 'NONE',  ( 0.000000000000000000, 0.000000000000000000, 1.000000000000000000 ) ) ;
#11361 = DIRECTION ( 'NONE',  ( 0.000000000000000000, -1.000000000000000000, 0.000000000000000000 ) ) ;
#11362 = APPLICATION_CONTEXT ( 'automotive_design' ) ;
#11363 = VERTEX_POINT ( 'NONE', #16054 ) ;
#11364 = ORIENTED_EDGE ( 'NONE', *, *, #6913, .T. ) ;
#11365 = ORIENTED_EDGE ( 'NONE', *, *, #21072, .F. ) ;
#11366 = ADVANCED_FACE ( 'NONE', ( #4344 ), #20714, .F. ) ;
#11367 = CIRCLE ( 'NONE', #4315, 44.99999999999999289 ) ;
#11368 = ORIENTED_EDGE ( 'NONE', *, *, #16484, .T. ) ;
#11369 = EDGE_LOOP ( 'NONE', ( #1348, #17384, #5135, #9533 ) ) ;
#11370 = DIRECTION ( 'NONE',  ( 0.000000000000000000, 0.000000000000000000, 1.000000000000000000 ) ) ;
#11371 = CIRCLE ( 'NONE', #18087, 45.00000000000000000 ) ;
#11372 = VERTEX_POINT ( 'NONE', #2574 ) ;
#11373 = CARTESIAN_POINT ( 'NONE',  ( -10.00000000000000000, 0.000000000000000000, 0.000000000000000000 ) ) ;
#11374 = CARTESIAN_POINT ( 'NONE',  ( 0.000000000000000000, 0.000000000000000000, 0.000000000000000000 ) ) ;
#11375 = AXIS2_PLACEMENT_3D ( 'NONE', #17673, #6184, #12688 ) ;
#11376 = EDGE_CURVE ( 'NONE', #9424, #14363, #19156, .T. ) ;
#11377 = DIRECTION ( 'NONE',  ( 0.000000000000000000, 0.000000000000000000, 1.000000000000000000 ) ) ;
#11378 = DIRECTION ( 'NONE',  ( 0.000000000000000000, 0.000000000000000000, 1.000000000000000000 ) ) ;
#11379 = DIRECTION ( 'NONE',  ( -1.000000000000000000, 0.000000000000000000, -0.000000000000000000 ) ) ;
#11380 = EDGE_CURVE ( 'NONE', #13798, #20540, #4376, .T. ) ;
#11381 = DIRECTION ( 'NONE',  ( -1.000000000000000000, 0.000000000000000000, 0.000000000000000000 ) ) ;
#11382 = CARTESIAN_POINT ( 'NONE',  ( 0.000000000000000000, -81.34229909304701778, 33.57723005635337898 ) ) ;
#11383 = CIRCLE ( 'NONE', #11748, 92.50100000000000477 ) ;
#11384 = ADVANCED_FACE ( 'NONE', ( #15737 ), #19381, .F. ) ;
#11385 = ORIENTED_EDGE ( 'NONE', *, *, #7605, .T. ) ;
#11386 = EDGE_CURVE ( 'NONE', #20466, #18737, #17396, .T. ) ;
#11387 = CARTESIAN_POINT ( 'NONE',  ( 0.000000000000000000, 0.000000000000000000, 0.000000000000000000 ) ) ;
#11388 = VECTOR ( 'NONE', #2539, 1000.000000000000000 ) ;
#11389 = VECTOR ( 'NONE', #2413, 1000.000000000000000 ) ;
#11390 = ORIENTED_EDGE ( 'NONE', *, *, #15131, .F. ) ;
#11391 = AXIS2_PLACEMENT_3D ( 'NONE', #21811, #6703, #13416 ) ;
#11392 = ORIENTED_EDGE ( 'NONE', *, *, #6956, .F. ) ;
#11393 = DIRECTION ( 'NONE',  ( 0.000000000000000000, 0.000000000000000000, -1.000000000000000000 ) ) ;
#11394 = FACE_OUTER_BOUND ( 'NONE', #13243, .T. ) ;
#11395 = AXIS2_PLACEMENT_3D ( 'NONE', #14148, #14254, #21006 ) ;
#11396 = ORIENTED_EDGE ( 'NONE', *, *, #7416, .T. ) ;
#11397 = LINE ( 'NONE', #18148, #8416 ) ;
#11398 = VERTEX_POINT ( 'NONE', #17623 ) ;
#11399 = ORIENTED_EDGE ( 'NONE', *, *, #5938, .T. ) ;
#11400 = SHAPE_DEFINITION_REPRESENTATION ( #21851, #2177 ) ;
#11401 = DIRECTION ( 'NONE',  ( -1.000000000000000000, 0.000000000000000000, 0.000000000000000000 ) ) ;
#11402 = VERTEX_POINT ( 'NONE', #920 ) ;
#11403 = LINE ( 'NONE', #7877, #19202 ) ;
#11404 = DIRECTION ( 'NONE',  ( 0.000000000000000000, 0.9848077530122074652, 0.1736481776669340227 ) ) ;
#11405 = AXIS2_PLACEMENT_3D ( 'NONE', #12684, #4289, #9656 ) ;
#11406 = CIRCLE ( 'NONE', #14573, 100.0000000000000000 ) ;
#11407 = DIRECTION ( 'NONE',  ( 0.000000000000000000, 0.000000000000000000, 1.000000000000000000 ) ) ;
#11408 = DIRECTION ( 'NONE',  ( 0.000000000000000000, 0.000000000000000000, -1.000000000000000000 ) ) ;
#11409 = CARTESIAN_POINT ( 'NONE',  ( 10.00000000000000000, 87.17509410653667601, -30.93441398372498341 ) ) ;
#11410 = LINE ( 'NONE', #18161, #8287 ) ;
#11411 = AXIS2_PLACEMENT_3D ( 'NONE', #16040, #9401, #9518 ) ;
#11412 = CARTESIAN_POINT ( 'NONE',  ( 10.00000000000000000, -89.12061559554314272, -24.77803214283632727 ) ) ;
#11413 = DIRECTION ( 'NONE',  ( 1.000000000000000000, 0.000000000000000000, 0.000000000000000000 ) ) ;
#11414 = CARTESIAN_POINT ( 'NONE',  ( 10.00000000000000000, 72.53479564998782791, 44.42851404693380601 ) ) ;
#11415 = AXIS2_PLACEMENT_3D ( 'NONE', #1898, #10509, #15593 ) ;
#11416 = ORIENTED_EDGE ( 'NONE', *, *, #14531, .T. ) ;
#11417 = CIRCLE ( 'NONE', #18491, 32.00000000000000000 ) ;
#11418 = VERTEX_POINT ( 'NONE', #14402 ) ;
#11419 = DIRECTION ( 'NONE',  ( 0.000000000000000000, 0.000000000000000000, 1.000000000000000000 ) ) ;
#11420 = AXIS2_PLACEMENT_3D ( 'NONE', #7782, #4902, #13287 ) ;
#11421 = ORIENTED_EDGE ( 'NONE', *, *, #410, .F. ) ;
#11422 = FACE_BOUND ( 'NONE', #12035, .T. ) ;
#11423 = PRODUCT ( 'planetary rotating cover', 'planetary rotating cover', '', ( #2895 ) ) ;
#11424 = VERTEX_POINT ( 'NONE', #7350 ) ;
#11425 = AXIS2_PLACEMENT_3D ( 'NONE', #17641, #7370, #15871 ) ;
#11426 = VERTEX_POINT ( 'NONE', #5793 ) ;
#11427 = ORIENTED_EDGE ( 'NONE', *, *, #298, .T. ) ;
#11428 = EDGE_LOOP ( 'NONE', ( #16508, #13240, #19123, #17575 ) ) ;
#11429 = LINE ( 'NONE', #6473, #21662 ) ;
#11430 = CARTESIAN_POINT ( 'NONE',  ( 10.00000000000000000, 61.33825423015778711, -69.23910433415882437 ) ) ;
#11431 = VERTEX_POINT ( 'NONE', #2475 ) ;
#11432 = CIRCLE ( 'NONE', #7921, 88.00000000000000000 ) ;
#11433 = DIRECTION ( 'NONE',  ( -1.000000000000000000, -0.000000000000000000, -0.000000000000000000 ) ) ;
#11434 = DIRECTION ( 'NONE',  ( 1.000000000000000000, -0.000000000000000000, -0.000000000000000000 ) ) ;
#11435 = DIRECTION ( 'NONE',  ( 0.000000000000000000, 0.9271838545667857590, 0.3746065934159159561 ) ) ;
#11436 = DIRECTION ( 'NONE',  ( 0.000000000000000000, 0.000000000000000000, -1.000000000000000000 ) ) ;
#11437 = CARTESIAN_POINT ( 'NONE',  ( 10.00000000000000000, -60.65655256511196569, -59.63197188857583342 ) ) ;
#11438 = CARTESIAN_POINT ( 'NONE',  ( -10.00000000000000000, 0.000000000000000000, 0.000000000000000000 ) ) ;
#11439 = UNCERTAINTY_MEASURE_WITH_UNIT (LENGTH_MEASURE( 1.000000000000000082E-05 ), #13771, 'distance_accuracy_value', 'NONE');
#11440 = AXIS2_PLACEMENT_3D ( 'NONE', #1633, #13779, #15209 ) ;
#11441 = EDGE_CURVE ( 'NONE', #10257, #5306, #21298, .T. ) ;
#11442 = ORIENTED_EDGE ( 'NONE', *, *, #21127, .F. ) ;
#11443 = CIRCLE ( 'NONE', #1913, 32.00000000000000000 ) ;
#11444 = LINE ( 'NONE', #12764, #15523 ) ;
#11445 = DIRECTION ( 'NONE',  ( 0.000000000000000000, -0.9702957262759988044, 0.2419218955996582376 ) ) ;
#11446 = EDGE_LOOP ( 'NONE', ( #17731, #10183, #20354, #16948 ) ) ;
#11447 = EDGE_CURVE ( 'NONE', #13770, #6615, #14078, .T. ) ;
#11448 = CYLINDRICAL_SURFACE ( 'NONE', #14713, 88.00000000000000000 ) ;
#11449 = ORIENTED_EDGE ( 'NONE', *, *, #16541, .T. ) ;
#11450 = AXIS2_PLACEMENT_3D ( 'NONE', #19007, #7084, #3753 ) ;
#11451 = DIRECTION ( 'NONE',  ( 0.000000000000000000, 0.000000000000000000, -1.000000000000000000 ) ) ;
#11452 = CIRCLE ( 'NONE', #912, 27.49900000000000588 ) ;
#11453 = CARTESIAN_POINT ( 'NONE',  ( -10.00000000000000000, 0.000000000000000000, 0.000000000000000000 ) ) ;
#11454 = ORIENTED_EDGE ( 'NONE', *, *, #143, .F. ) ;
#11455 = DIRECTION ( 'NONE',  ( 1.000000000000000000, -0.000000000000000000, -0.000000000000000000 ) ) ;
#11456 = VECTOR ( 'NONE', #18622, 1000.000000000000000 ) ;
#11457 = ORIENTED_EDGE ( 'NONE', *, *, #10298, .F. ) ;
#11458 = ORIENTED_EDGE ( 'NONE', *, *, #14624, .F. ) ;
#11459 = DIRECTION ( 'NONE',  ( 0.000000000000000000, 1.000000000000000000, -0.000000000000000000 ) ) ;
#11460 = VECTOR ( 'NONE', #16438, 1000.000000000000000 ) ;
#11461 = EDGE_LOOP ( 'NONE', ( #1589, #1810, #21317, #1653 ) ) ;
#11462 = DIRECTION ( 'NONE',  ( -1.000000000000000000, -0.000000000000000000, -0.000000000000000000 ) ) ;
#11463 = CARTESIAN_POINT ( 'NONE',  ( 10.00000000000000000, -2.481790431839894673, 92.46770094066590673 ) ) ;
#11464 = DIRECTION ( 'NONE',  ( -1.000000000000000000, 0.000000000000000000, 0.000000000000000000 ) ) ;
#11465 = DIRECTION ( 'NONE',  ( 0.000000000000000000, 0.000000000000000000, 1.000000000000000000 ) ) ;
#11466 = DIRECTION ( 'NONE',  ( 1.000000000000000000, 0.000000000000000000, 0.000000000000000000 ) ) ;
#11467 = AXIS2_PLACEMENT_3D ( 'NONE', #17779, #19653, #7728 ) ;
#11468 = EDGE_CURVE ( 'NONE', #536, #155, #11773, .T. ) ;
#11469 = DIRECTION ( 'NONE',  ( -1.000000000000000000, -0.000000000000000000, -0.000000000000000000 ) ) ;
#11470 = EDGE_CURVE ( 'NONE', #2155, #5782, #16356, .T. ) ;
#11471 = DIRECTION ( 'NONE',  ( 0.000000000000000000, 0.000000000000000000, 1.000000000000000000 ) ) ;
#11472 = CIRCLE ( 'NONE', #14655, 88.00000000000000000 ) ;
#11473 = DIRECTION ( 'NONE',  ( 1.000000000000000000, 0.000000000000000000, 0.000000000000000000 ) ) ;
#11474 = ADVANCED_BREP_SHAPE_REPRESENTATION ( '', ( #6279, #15567 ), #19793 ) ;
#11475 = CARTESIAN_POINT ( 'NONE',  ( 10.00000000000000000, 87.92084725184953697, -3.731570516142035387 ) ) ;
#11476 = CARTESIAN_POINT ( 'NONE',  ( 0.000000000000000000, -17.83210509884626660, -21.83428559348779530 ) ) ;
#11477 = VECTOR ( 'NONE', #3071, 1000.000000000000000 ) ;
#11478 = DIRECTION ( 'NONE',  ( 0.000000000000000000, 0.000000000000000000, 1.000000000000000000 ) ) ;
#11479 = ORIENTED_EDGE ( 'NONE', *, *, #11165, .F. ) ;
#11480 = ORIENTED_EDGE ( 'NONE', *, *, #10648, .T. ) ;
#11481 = AXIS2_PLACEMENT_3D ( 'NONE', #9544, #21596, #21388 ) ;
#11482 = EDGE_LOOP ( 'NONE', ( #6900, #9974, #13104, #13971 ) ) ;
#11483 = EDGE_CURVE ( 'NONE', #4745, #10738, #18136, .T. ) ;
#11484 = ORIENTED_EDGE ( 'NONE', *, *, #10580, .T. ) ;
#11485 = AXIS2_PLACEMENT_3D ( 'NONE', #10753, #17951, #15852 ) ;
#11486 = VECTOR ( 'NONE', #20530, 1000.000000000000000 ) ;
#11487 = CIRCLE ( 'NONE', #1966, 44.99999999999998579 ) ;
#11488 = CIRCLE ( 'NONE', #10784, 92.50100000000000477 ) ;
#11489 = ORIENTED_EDGE ( 'NONE', *, *, #17859, .T. ) ;
#11490 = EDGE_CURVE ( 'NONE', #3061, #18563, #16004, .T. ) ;
#11491 = AXIS2_PLACEMENT_3D ( 'NONE', #19671, #4647, #16248 ) ;
#11492 = DIRECTION ( 'NONE',  ( 0.000000000000000000, 0.6946583704589934793, 0.7193398003386547446 ) ) ;
#11493 = EDGE_LOOP ( 'NONE', ( #19991, #9516, #21130, #5232 ) ) ;
#11494 = CARTESIAN_POINT ( 'NONE',  ( 10.00000000000000000, -77.39385041987125646, -35.28996114464684553 ) ) ;
#11495 = CARTESIAN_POINT ( 'NONE',  ( 10.00000000000000000, -83.89484365856928605, 26.56417150042919673 ) ) ;
#11496 = EDGE_CURVE ( 'NONE', #9954, #1185, #7203, .T. ) ;
#11497 = DIRECTION ( 'NONE',  ( 0.000000000000000000, 0.000000000000000000, 1.000000000000000000 ) ) ;
#11498 = CARTESIAN_POINT ( 'NONE',  ( 10.00000000000000000, -26.27606311335958011, 10.21217444509402661 ) ) ;
#11499 = CARTESIAN_POINT ( 'NONE',  ( 0.000000000000000000, 0.000000000000000000, 0.000000000000000000 ) ) ;
#11500 = ADVANCED_FACE ( 'NONE', ( #4460, #9412 ), #6357, .T. ) ;
#11501 = DIRECTION ( 'NONE',  ( 0.000000000000000000, 0.000000000000000000, 1.000000000000000000 ) ) ;
#11502 = CARTESIAN_POINT ( 'NONE',  ( 10.00000000000000000, 45.60224695560681596, -80.47900393021679122 ) ) ;
#11503 = EDGE_CURVE ( 'NONE', #16515, #9022, #12955, .T. ) ;
#11504 = CIRCLE ( 'NONE', #11848, 44.99999999999999289 ) ;
#11505 = VERTEX_POINT ( 'NONE', #19707 ) ;
#11506 = CIRCLE ( 'NONE', #5178, 11.99999999999999822 ) ;
#11507 = CARTESIAN_POINT ( 'NONE',  ( 10.00000000000000000, 8.925965667928872804, 92.06933331948788179 ) ) ;
#11508 = AXIS2_PLACEMENT_3D ( 'NONE', #12453, #9240, #17444 ) ;
#11509 = VERTEX_POINT ( 'NONE', #9527 ) ;
#11510 = ORIENTED_EDGE ( 'NONE', *, *, #3710, .F. ) ;
#11511 = EDGE_CURVE ( 'NONE', #14361, #17102, #14729, .T. ) ;
#11512 = CARTESIAN_POINT ( 'NONE',  ( 0.000000000000000000, 0.000000000000000000, 0.000000000000000000 ) ) ;
#11513 = ORIENTED_EDGE ( 'NONE', *, *, #9969, .F. ) ;
#11514 = CYLINDRICAL_SURFACE ( 'NONE', #17946, 45.00000000000000000 ) ;
#11515 = ORIENTED_EDGE ( 'NONE', *, *, #782, .T. ) ;
#11516 = ADVANCED_FACE ( 'NONE', ( #1143 ), #7885, .F. ) ;
#11517 = EDGE_LOOP ( 'NONE', ( #8370, #669, #6827, #2591 ) ) ;
#11518 = CARTESIAN_POINT ( 'NONE',  ( 10.00000000000000000, -84.79630770241089976, 6.691460262315113816 ) ) ;
#11519 = ORIENTED_EDGE ( 'NONE', *, *, #1792, .F. ) ;
#11520 = AXIS2_PLACEMENT_3D ( 'NONE', #19221, #4088, #4294 ) ;
#11521 = DIRECTION ( 'NONE',  ( 1.000000000000000000, 0.000000000000000000, 0.000000000000000000 ) ) ;
#11522 = CIRCLE ( 'NONE', #4821, 11.99999999999999822 ) ;
#11523 = DIRECTION ( 'NONE',  ( 0.000000000000000000, 0.000000000000000000, -1.000000000000000000 ) ) ;
#11524 = EDGE_CURVE ( 'NONE', #16840, #16161, #8602, .T. ) ;
#11525 = VECTOR ( 'NONE', #8811, 1000.000000000000000 ) ;
#11526 = FACE_OUTER_BOUND ( 'NONE', #10908, .T. ) ;
#11527 = CYLINDRICAL_SURFACE ( 'NONE', #20405, 45.00000000000000000 ) ;
#11528 = DIRECTION ( 'NONE',  ( -1.000000000000000000, 0.000000000000000000, -0.000000000000000000 ) ) ;
#11529 = CARTESIAN_POINT ( 'NONE',  ( 0.000000000000000000, 0.000000000000000000, 0.000000000000000000 ) ) ;
#11530 = CYLINDRICAL_SURFACE ( 'NONE', #12530, 88.00000000000000000 ) ;
#11531 = DIRECTION ( 'NONE',  ( 0.000000000000000000, -0.7880107536067275653, 0.6156614753256510753 ) ) ;
#11532 = ADVANCED_FACE ( 'NONE', ( #3129 ), #21477, .F. ) ;
#11533 = EDGE_LOOP ( 'NONE', ( #18231, #15251, #2390, #10798 ) ) ;
#11534 = VECTOR ( 'NONE', #16800, 1000.000000000000000 ) ;
#11535 = AXIS2_PLACEMENT_3D ( 'NONE', #20495, #7230, #6805 ) ;
#11536 = AXIS2_PLACEMENT_3D ( 'NONE', #4964, #18343, #3192 ) ;
#11537 = AXIS2_PLACEMENT_3D ( 'NONE', #17455, #7614, #19323 ) ;
#11538 = DIRECTION ( 'NONE',  ( -1.000000000000000000, -0.000000000000000000, -0.000000000000000000 ) ) ;
#11539 = DIRECTION ( 'NONE',  ( 0.000000000000000000, 0.000000000000000000, 1.000000000000000000 ) ) ;
#11540 = VERTEX_POINT ( 'NONE', #14515 ) ;
#11541 = CARTESIAN_POINT ( 'NONE',  ( 10.00000000000000000, -26.27606311335958011, 10.21217444509402661 ) ) ;
#11542 = ADVANCED_FACE ( 'NONE', ( #2808 ), #9632, .F. ) ;
#11543 = VERTEX_POINT ( 'NONE', #20035 ) ;
#11544 = VERTEX_POINT ( 'NONE', #16385 ) ;
#11545 = CARTESIAN_POINT ( 'NONE',  ( 10.00000000000000000, -78.80192417387952730, 39.16958956249271040 ) ) ;
#11546 = EDGE_LOOP ( 'NONE', ( #19584, #14472, #16160, #12053 ) ) ;
#11547 = ORIENTED_EDGE ( 'NONE', *, *, #7755, .T. ) ;
#11548 = DIRECTION ( 'NONE',  ( 0.000000000000000000, 0.5877852522924743583, -0.8090169943749465631 ) ) ;
#11549 = DIRECTION ( 'NONE',  ( 0.000000000000000000, 1.000000000000000000, 0.000000000000000000 ) ) ;
#11550 = EDGE_LOOP ( 'NONE', ( #21315, #14593, #16042, #4100 ) ) ;
#11551 = EDGE_CURVE ( 'NONE', #5152, #3214, #15662, .T. ) ;
#11552 = VECTOR ( 'NONE', #21306, 1000.000000000000000 ) ;
#11553 = CYLINDRICAL_SURFACE ( 'NONE', #20619, 88.00000000000000000 ) ;
#11554 = DIRECTION ( 'NONE',  ( 0.000000000000000000, -0.8987940462991710344, 0.4383711467890689106 ) ) ;
#11555 = AXIS2_PLACEMENT_3D ( 'NONE', #4170, #16207, #10903 ) ;
#11556 = DIRECTION ( 'NONE',  ( 0.000000000000000000, 1.224646799147362821E-16, 1.000000000000000000 ) ) ;
#11557 = DIRECTION ( 'NONE',  ( 0.000000000000000000, 0.000000000000000000, 1.000000000000000000 ) ) ;
#11558 = CIRCLE ( 'NONE', #1333, 12.00000000000000178 ) ;
#11559 = CARTESIAN_POINT ( 'NONE',  ( 0.000000000000000000, 47.19205848891868271, -74.27590198428072199 ) ) ;
#11560 = FACE_OUTER_BOUND ( 'NONE', #7009, .T. ) ;
#11561 = EDGE_LOOP ( 'NONE', ( #13300, #6058, #21287, #217 ) ) ;
#11562 = LINE ( 'NONE', #6276, #1760 ) ;
#11563 = DIRECTION ( 'NONE',  ( 1.000000000000000000, 0.000000000000000000, 0.000000000000000000 ) ) ;
#11564 = ORIENTED_EDGE ( 'NONE', *, *, #7905, .F. ) ;
#11565 = DIRECTION ( 'NONE',  ( -1.000000000000000000, -0.000000000000000000, 0.000000000000000000 ) ) ;
#11566 = ORIENTED_EDGE ( 'NONE', *, *, #12580, .F. ) ;
#11567 = AXIS2_PLACEMENT_3D ( 'NONE', #13825, #8850, #14039 ) ;
#11568 = CARTESIAN_POINT ( 'NONE',  ( 5.000000000000000888, 6.063030049135493371, -31.42037024962118608 ) ) ;
#11569 = AXIS2_PLACEMENT_3D ( 'NONE', #2600, #19292, #4157 ) ;
#11570 = CARTESIAN_POINT ( 'NONE',  ( 10.00000000000000000, -14.53731623274912366, -23.34226719384920656 ) ) ;
#11571 = VECTOR ( 'NONE', #17725, 1000.000000000000000 ) ;
#11572 = EDGE_CURVE ( 'NONE', #20049, #9164, #1257, .T. ) ;
#11573 = EDGE_LOOP ( 'NONE', ( #21209, #14828, #14338, #10350, #11892, #10501, #8689, #1681, #16477, #16647, #450, #4451, #18672, #20860, #20643, #21426, #15609, #7819, #748, #21433, #5038, #3252, #14856, #10035, #11214, #5726, #18846, #8767, #21612, #18718, #15228, #8454, #2025, #3577, #9587, #17882, #9085, #12261, #2811, #11489, #2318, #5667, #5890, #905, #17283, #4905, #19963, #13763, #9540, #10795, #5246, #16844, #10381, #7811, #2893, #18526, #2490, #2185, #12096, #6460, #2891, #7927, #15474, #16906, #11316, #9398, #17910, #10706, #4466, #8518, #152, #6791, #1059, #19173, #17442, #8394, #3310, #20401, #16292, #19074, #18070, #19997, #13604, #17144, #19186, #11346, #17404, #5210, #8280, #16818, #4854, #4774, #13572, #7659, #4883, #14931, #14273, #4280, #17630, #12157, #20628, #16552, #16568, #16454, #20705, #10911, #8740, #13733, #9313, #15796, #482, #7983, #19457, #3903, #13418, #7949, #1015, #9033, #1302, #3108, #17823, #21108, #3389, #5272, #7415, #18208, #3902, #13270, #3974, #7673, #9000, #18775, #17409, #8477, #21781, #14780, #1732, #18769, #19420, #14011, #17922, #506, #19908, #20236, #2798, #16452, #11037, #7791, #4173, #15115, #5869, #2739, #2085, #11421, #13061, #20856, #16935, #7488, #2868, #21451, #1590, #8037, #3601, #12262, #18791, #9235, #3627, #9161, #12118, #1512, #6812, #7256, #8948, #7587, #4835, #4028, #21213, #12970, #8894, #19856, #6313, #10451, #4744, #6173, #17584, #2007, #2400, #6213, #21056, #16969, #6439, #5052, #5979, #10378, #5540, #21558, #17853, #3038, #15408, #18593, #11701, #400, #9539, #3927, #11229, #6830, #19011, #16399, #19494, #1827, #3853, #16745, #11128, #5669, #13737, #14142, #15022, #5082, #6828, #4718, #8145, #20265, #8178, #19794, #1557, #7304, #16241, #17023, #6964, #12963, #1984, #16129, #8719, #19823, #2053, #15386, #20945, #3384, #9666, #13519, #11322, #16243, #21801, #21021, #3762, #9764, #9139, #7257, #10659, #11872, #16190, #15739, #9328, #1501, #14652, #8127, #5488, #9184, #4175, #5119, #11776, #8552, #10687, #2435, #12722, #10871, #6163, #21314, #13413, #9028, #15452, #19464, #13138, #20155, #18269, #2593, #2051, #6112, #18149, #4296, #11139, #17768, #4126, #20672, #5532, #8525, #9811, #20834, #335, #10082, #11392, #19805, #7458, #15012, #4991, #8626, #8193, #3174, #10216, #16256, #19487, #5197, #5552, #20108, #11953, #10530, #10060, #14504, #21041, #17785, #11014, #16101, #15422, #12397, #12244, #10236, #3447, #7245, #8973, #19750, #8845, #5611, #9278, #10744, #5596, #10606, #20272, #7868, #17029, #18589, #12794, #7303, #3959, #8756, #20189, #18428, #2887, #18797, #6939, #18036, #19342, #3323, #17989, #9928, #6082, #17073, #21805, #6850, #6079, #9058, #1164, #18722, #728, #6467, #9346, #3679, #13987, #2649, #17331, #10085, #21545, #2721, #618 ) ) ;
#11574 = DIRECTION ( 'NONE',  ( 0.000000000000000000, -1.079383496163347022E-14, -1.000000000000000000 ) ) ;
#11575 = VERTEX_POINT ( 'NONE', #18163 ) ;
#11576 = ORIENTED_EDGE ( 'NONE', *, *, #16307, .F. ) ;
#11577 = CARTESIAN_POINT ( 'NONE',  ( 10.00000000000000000, -37.96946988134122591, -76.11510229470897571 ) ) ;
#11578 = VERTEX_POINT ( 'NONE', #3022 ) ;
#11579 = CIRCLE ( 'NONE', #17934, 92.50099999999999056 ) ;
#11580 = DIRECTION ( 'NONE',  ( 0.000000000000000000, 0.000000000000000000, 1.000000000000000000 ) ) ;
#11581 = DIRECTION ( 'NONE',  ( 1.000000000000000000, 0.000000000000000000, 0.000000000000000000 ) ) ;
#11582 = DIRECTION ( 'NONE',  ( 1.000000000000000000, -0.000000000000000000, -0.000000000000000000 ) ) ;
#11583 = DIRECTION ( 'NONE',  ( 0.000000000000000000, -0.9510565162951503115, -0.3090169943749573878 ) ) ;
#11584 = CIRCLE ( 'NONE', #13694, 44.99999999999999289 ) ;
#11585 = AXIS2_PLACEMENT_3D ( 'NONE', #9626, #8205, #19700 ) ;
#11586 = AXIS2_PLACEMENT_3D ( 'NONE', #18817, #5343, #369 ) ;
#11587 = CARTESIAN_POINT ( 'NONE',  ( 0.000000000000000000, 52.34334029047876413, 76.26670130689501548 ) ) ;
#11588 = DIRECTION ( 'NONE',  ( 0.000000000000000000, -0.8660254037844431485, 0.4999999999999919509 ) ) ;
#11589 = AXIS2_PLACEMENT_3D ( 'NONE', #21685, #21797, #14944 ) ;
#11590 = CARTESIAN_POINT ( 'NONE',  ( 5.000000000000000000, -24.17932380791704716, -20.96092317127029503 ) ) ;
#11591 = DIRECTION ( 'NONE',  ( -1.000000000000000000, -0.000000000000000000, 0.000000000000000000 ) ) ;
#11592 = CARTESIAN_POINT ( 'NONE',  ( 0.000000000000000000, 81.32027326007866463, 44.08455690949082850 ) ) ;
#11593 = ORIENTED_EDGE ( 'NONE', *, *, #15301, .F. ) ;
#11594 = VERTEX_POINT ( 'NONE', #16499 ) ;
#11595 = ORIENTED_EDGE ( 'NONE', *, *, #3689, .F. ) ;
#11596 = CIRCLE ( 'NONE', #17593, 44.99999999999998579 ) ;
#11597 = ORIENTED_EDGE ( 'NONE', *, *, #20918, .F. ) ;
#11598 = EDGE_CURVE ( 'NONE', #11575, #17610, #3661, .T. ) ;
#11599 = VECTOR ( 'NONE', #2456, 1000.000000000000000 ) ;
#11600 = CIRCLE ( 'NONE', #2077, 88.00000000000000000 ) ;
#11601 = CIRCLE ( 'NONE', #16887, 44.99999999999999289 ) ;
#11602 = AXIS2_PLACEMENT_3D ( 'NONE', #20823, #8880, #7126 ) ;
#11603 = CIRCLE ( 'NONE', #4536, 32.00000000000000000 ) ;
#11604 = VERTEX_POINT ( 'NONE', #8109 ) ;
#11605 = CARTESIAN_POINT ( 'NONE',  ( 8.899999999999991473, 0.000000000000000000, 0.000000000000000000 ) ) ;
#11606 = ORIENTED_EDGE ( 'NONE', *, *, #6699, .T. ) ;
#11607 = CARTESIAN_POINT ( 'NONE',  ( 7.395800000000001262, 1.407128969394701661E-14, 114.9007999999999896 ) ) ;
#11608 = DIRECTION ( 'NONE',  ( 0.000000000000000000, 0.000000000000000000, 1.000000000000000000 ) ) ;
#11609 = ADVANCED_FACE ( 'NONE', ( #13170, #12844 ), #16605, .T. ) ;
#11610 = DIRECTION ( 'NONE',  ( -1.000000000000000000, -0.000000000000000000, 0.000000000000000000 ) ) ;
#11611 = LINE ( 'NONE', #18131, #4899 ) ;
#11612 = LINE ( 'NONE', #8080, #5538 ) ;
#11613 = EDGE_CURVE ( 'NONE', #20211, #2977, #18845, .T. ) ;
#11614 = DIRECTION ( 'NONE',  ( 0.000000000000000000, 0.2079116908177599254, -0.9781476007338055778 ) ) ;
#11615 = CIRCLE ( 'NONE', #19367, 6.887500000000022382 ) ;
#11616 = AXIS2_PLACEMENT_3D ( 'NONE', #4829, #19965, #70 ) ;
#11617 = AXIS2_PLACEMENT_3D ( 'NONE', #9784, #16311, #961 ) ;
#11618 = ORIENTED_EDGE ( 'NONE', *, *, #1375, .F. ) ;
#11619 = AXIS2_PLACEMENT_3D ( 'NONE', #5090, #10376, #7181 ) ;
#11620 = CARTESIAN_POINT ( 'NONE',  ( 10.00000000000000000, -84.12297548659729785, 12.59025161326973397 ) ) ;
#11621 = ORIENTED_EDGE ( 'NONE', *, *, #19058, .F. ) ;
#11622 = ORIENTED_EDGE ( 'NONE', *, *, #17705, .F. ) ;
#11623 = DIRECTION ( 'NONE',  ( 1.000000000000000000, 0.000000000000000000, 0.000000000000000000 ) ) ;
#11624 = EDGE_CURVE ( 'NONE', #16392, #8251, #10359, .T. ) ;
#11625 = EDGE_LOOP ( 'NONE', ( #9322, #4032, #11787, #2252 ) ) ;
#11626 = ADVANCED_FACE ( 'NONE', ( #5114 ), #18809, .F. ) ;
#11627 = EDGE_CURVE ( 'NONE', #21052, #15273, #13832, .T. ) ;
#11628 = DIRECTION ( 'NONE',  ( 0.000000000000000000, 2.621359919253842577E-15, -1.000000000000000000 ) ) ;
#11629 = ORIENTED_EDGE ( 'NONE', *, *, #13083, .T. ) ;
#11630 = ORIENTED_EDGE ( 'NONE', *, *, #14325, .F. ) ;
#11631 = ITEM_DEFINED_TRANSFORMATION ( 'NONE', 'NONE', #15580,  #15567 ) ;
#11632 = CARTESIAN_POINT ( 'NONE',  ( 5.000000000000000000, -28.00896854771981737, -15.47571261340952020 ) ) ;
#11633 = EDGE_CURVE ( 'NONE', #610, #16361, #14592, .T. ) ;
#11634 = ORIENTED_EDGE ( 'NONE', *, *, #20464, .T. ) ;
#11635 = AXIS2_PLACEMENT_3D ( 'NONE', #21378, #7677, #6140 ) ;
#11636 = DIRECTION ( 'NONE',  ( -1.000000000000000000, 0.000000000000000000, 0.000000000000000000 ) ) ;
#11637 = AXIS2_PLACEMENT_3D ( 'NONE', #20319, #8492, #5181 ) ;
#11638 = CARTESIAN_POINT ( 'NONE',  ( 10.00000000000000000, 19.85071254963777676, 20.01672328094538145 ) ) ;
#11639 = DIRECTION ( 'NONE',  ( -1.000000000000000000, -0.000000000000000000, 0.000000000000000000 ) ) ;
#11640 = CARTESIAN_POINT ( 'NONE',  ( 0.000000000000000000, 0.000000000000000000, -3.000000000000000000 ) ) ;
#11641 = CARTESIAN_POINT ( 'NONE',  ( 10.00000000000000000, 0.000000000000000000, 0.000000000000000000 ) ) ;
#11642 = DIRECTION ( 'NONE',  ( -1.000000000000000000, -0.000000000000000000, -0.000000000000000000 ) ) ;
#11643 = CARTESIAN_POINT ( 'NONE',  ( 10.00000000000000000, -72.53479564998815476, 44.42851404693331574 ) ) ;
#11644 = ADVANCED_FACE ( 'NONE', ( #18599 ), #10195, .T. ) ;
#11645 = LINE ( 'NONE', #18389, #13700 ) ;
#11646 = ORIENTED_EDGE ( 'NONE', *, *, #5987, .T. ) ;
#11647 = ADVANCED_FACE ( 'NONE', ( #15162 ), #9962, .T. ) ;
#11648 = PRESENTATION_LAYER_ASSIGNMENT (  '', '', ( #9156 ) ) ;
#11649 = DIRECTION ( 'NONE',  ( 1.000000000000000000, 0.000000000000000000, 0.000000000000000000 ) ) ;
#11650 = CARTESIAN_POINT ( 'NONE',  ( 0.000000000000000000, -27.40684453873955562, -16.51862198942037097 ) ) ;
#11651 = VERTEX_POINT ( 'NONE', #21795 ) ;
#11652 = DIRECTION ( 'NONE',  ( 0.000000000000000000, 0.7431448254773909134, 0.6691306063588619013 ) ) ;
#11653 = VERTEX_POINT ( 'NONE', #20477 ) ;
#11654 = SHAPE_REPRESENTATION_RELATIONSHIP ( 'NONE' , 'NONE' ,  #16445, #6478 ) ;
#11655 = VERTEX_POINT ( 'NONE', #3230 ) ;
#11656 = CARTESIAN_POINT ( 'NONE',  ( -90.00000000000000000, 0.000000000000000000, 0.000000000000000000 ) ) ;
#11657 = EDGE_CURVE ( 'NONE', #4799, #5374, #1189, .T. ) ;
#11658 = VERTEX_POINT ( 'NONE', #16825 ) ;
#11659 = ORIENTED_EDGE ( 'NONE', *, *, #20008, .T. ) ;
#11660 = DIRECTION ( 'NONE',  ( 0.000000000000000000, 0.000000000000000000, 1.000000000000000000 ) ) ;
#11661 = CARTESIAN_POINT ( 'NONE',  ( 5.000000000000000888, 13.56333590714014825, 28.98337314858439839 ) ) ;
#11662 = EDGE_LOOP ( 'NONE', ( #7127, #3824, #17189, #7095 ) ) ;
#11663 = DIRECTION ( 'NONE',  ( 0.000000000000000000, 0.000000000000000000, -1.000000000000000000 ) ) ;
#11664 = DIRECTION ( 'NONE',  ( 0.000000000000000000, 0.000000000000000000, 1.000000000000000000 ) ) ;
#11665 = DIRECTION ( 'NONE',  ( 0.000000000000000000, -0.7431448254774000173, 0.6691306063588517983 ) ) ;
#11666 = CIRCLE ( 'NONE', #12366, 88.00000000000000000 ) ;
#11667 = LINE ( 'NONE', #18413, #13191 ) ;
#11668 = CARTESIAN_POINT ( 'NONE',  ( 10.00000000000000000, 0.000000000000000000, 0.000000000000000000 ) ) ;
#11669 = CARTESIAN_POINT ( 'NONE',  ( 0.000000000000000000, -3.974475837765555575, 92.41557521768190497 ) ) ;
#11670 = UNCERTAINTY_MEASURE_WITH_UNIT (LENGTH_MEASURE( 1.000000000000000082E-05 ), #16722, 'distance_accuracy_value', 'NONE');
#11671 = EDGE_CURVE ( 'NONE', #8420, #11651, #8261, .T. ) ;
#11672 = EDGE_LOOP ( 'NONE', ( #18344, #14501, #194, #3308 ) ) ;
#11673 = EDGE_CURVE ( 'NONE', #10646, #5499, #8955, .T. ) ;
#11674 = CARTESIAN_POINT ( 'NONE',  ( 0.000000000000000000, -6.797690662954623875, -87.73705831432221203 ) ) ;
#11675 = DIRECTION ( 'NONE',  ( 0.000000000000000000, 0.000000000000000000, 1.000000000000000000 ) ) ;
#11676 = ORIENTED_EDGE ( 'NONE', *, *, #9230, .F. ) ;
#11677 = EDGE_CURVE ( 'NONE', #14192, #389, #8440, .T. ) ;
#11678 = ADVANCED_FACE ( 'NONE', ( #8536, #15262 ), #139, .T. ) ;
#11679 = CARTESIAN_POINT ( 'NONE',  ( 10.00000000000000000, 84.19736439813857487, -38.30455363800848545 ) ) ;
#11680 = ORIENTED_EDGE ( 'NONE', *, *, #12966, .T. ) ;
#11681 =( LENGTH_UNIT ( ) NAMED_UNIT ( * ) SI_UNIT ( .MILLI., .METRE. ) );
#11682 = FACE_OUTER_BOUND ( 'NONE', #12730, .T. ) ;
#11683 = ORIENTED_EDGE ( 'NONE', *, *, #14627, .T. ) ;
#11684 = DIRECTION ( 'NONE',  ( 0.000000000000000000, 0.000000000000000000, 1.000000000000000000 ) ) ;
#11685 = ORIENTED_EDGE ( 'NONE', *, *, #3681, .T. ) ;
#11686 = EDGE_LOOP ( 'NONE', ( #12974, #21320, #11828, #21511 ) ) ;
#11687 = DIRECTION ( 'NONE',  ( -1.000000000000000000, 0.000000000000000000, -0.000000000000000000 ) ) ;
#11688 = ORIENTED_EDGE ( 'NONE', *, *, #19713, .T. ) ;
#11689 = FACE_OUTER_BOUND ( 'NONE', #5810, .T. ) ;
#11690 = AXIS2_PLACEMENT_3D ( 'NONE', #6714, #13428, #20172 ) ;
#11691 = CARTESIAN_POINT ( 'NONE',  ( -7.440711023145607506, 0.000000000000000000, 0.000000000000000000 ) ) ;
#11692 = DIRECTION ( 'NONE',  ( 0.000000000000000000, 0.000000000000000000, 1.000000000000000000 ) ) ;
#11693 = DIRECTION ( 'NONE',  ( 1.000000000000000000, -0.000000000000000000, -0.000000000000000000 ) ) ;
#11694 = DIRECTION ( 'NONE',  ( 0.000000000000000000, 0.000000000000000000, -1.000000000000000000 ) ) ;
#11695 = LINE ( 'NONE', #1640, #18627 ) ;
#11696 = DIRECTION ( 'NONE',  ( 0.000000000000000000, 0.000000000000000000, 1.000000000000000000 ) ) ;
#11697 = STYLED_ITEM ( 'NONE', ( #12420 ), #11474 ) ;
#11698 = CARTESIAN_POINT ( 'NONE',  ( -10.00000000000000000, 0.000000000000000000, 0.000000000000000000 ) ) ;
#11699 = DIRECTION ( 'NONE',  ( 0.000000000000000000, 0.000000000000000000, 1.000000000000000000 ) ) ;
#11700 = CARTESIAN_POINT ( 'NONE',  ( 0.000000000000000000, -80.18694381077088451, -28.37681241246736974 ) ) ;
#11701 = ORIENTED_EDGE ( 'NONE', *, *, #10268, .T. ) ;
#11702 = DIRECTION ( 'NONE',  ( 0.000000000000000000, 1.224646799147355426E-16, 1.000000000000000000 ) ) ;
#11703 = ORIENTED_EDGE ( 'NONE', *, *, #18226, .F. ) ;
#11704 = ORIENTED_EDGE ( 'NONE', *, *, #6376, .T. ) ;
#11705 = ORIENTED_EDGE ( 'NONE', *, *, #2464, .T. ) ;
#11706 = AXIS2_PLACEMENT_3D ( 'NONE', #21022, #14718, #7772 ) ;
#11707 = ORIENTED_EDGE ( 'NONE', *, *, #14983, .T. ) ;
#11708 = FACE_OUTER_BOUND ( 'NONE', #3684, .T. ) ;
#11709 = ORIENTED_EDGE ( 'NONE', *, *, #7529, .F. ) ;
#11710 = DIRECTION ( 'NONE',  ( 0.000000000000000000, 0.000000000000000000, -1.000000000000000000 ) ) ;
#11711 = DIRECTION ( 'NONE',  ( 1.000000000000000000, 0.000000000000000000, 0.000000000000000000 ) ) ;
#11712 = CARTESIAN_POINT ( 'NONE',  ( 0.000000000000000000, 56.35896156214949571, 73.34918167666329225 ) ) ;
#11713 = CARTESIAN_POINT ( 'NONE',  ( 10.00000000000000000, -26.69209308833512395, 6.612652082459228531 ) ) ;
#11714 = DIRECTION ( 'NONE',  ( -1.000000000000000000, 0.000000000000000000, -0.000000000000000000 ) ) ;
#11715 = FACE_OUTER_BOUND ( 'NONE', #19391, .T. ) ;
#11716 = EDGE_CURVE ( 'NONE', #21723, #15150, #17042, .T. ) ;
#11717 = ORIENTED_EDGE ( 'NONE', *, *, #21665, .F. ) ;
#11718 = CARTESIAN_POINT ( 'NONE',  ( 10.00000000000000000, 78.01214607583752070, 33.90124636420136994 ) ) ;
#11719 = VECTOR ( 'NONE', #16016, 1000.000000000000000 ) ;
#11720 = VERTEX_POINT ( 'NONE', #3567 ) ;
#11721 = EDGE_CURVE ( 'NONE', #18379, #19278, #17423, .T. ) ;
#11722 = ORIENTED_EDGE ( 'NONE', *, *, #15518, .F. ) ;
#11723 = DIRECTION ( 'NONE',  ( 0.000000000000000000, 0.000000000000000000, -1.000000000000000000 ) ) ;
#11724 = VECTOR ( 'NONE', #17911, 1000.000000000000000 ) ;
#11725 = ORIENTED_EDGE ( 'NONE', *, *, #21637, .T. ) ;
#11726 = CARTESIAN_POINT ( 'NONE',  ( 10.00000000000000000, 40.72878876293257377, -78.00747250042405767 ) ) ;
#11727 = VERTEX_POINT ( 'NONE', #8638 ) ;
#11728 = ORIENTED_EDGE ( 'NONE', *, *, #8914, .T. ) ;
#11729 = CARTESIAN_POINT ( 'NONE',  ( 10.00000000000000000, -75.27139873020847460, -53.76477968147890607 ) ) ;
#11730 = ORIENTED_EDGE ( 'NONE', *, *, #15533, .F. ) ;
#11731 = CARTESIAN_POINT ( 'NONE',  ( 0.000000000000000000, -28.00896854771981737, -15.47571261340952020 ) ) ;
#11732 = CIRCLE ( 'NONE', #13476, 92.50100000000001899 ) ;
#11733 = LINE ( 'NONE', #13724, #15006 ) ;
#11734 = FACE_OUTER_BOUND ( 'NONE', #8312, .T. ) ;
#11735 = LINE ( 'NONE', #10510, #12916 ) ;
#11736 = CARTESIAN_POINT ( 'NONE',  ( 10.00000000000000000, 23.57863763525720202, 15.45211464167672588 ) ) ;
#11737 = CYLINDRICAL_SURFACE ( 'NONE', #18199, 44.99999999999999289 ) ;
#11738 = LINE ( 'NONE', #6688, #11218 ) ;
#11739 = VECTOR ( 'NONE', #17454, 1000.000000000000000 ) ;
#11740 = EDGE_CURVE ( 'NONE', #7767, #6657, #134, .T. ) ;
#11741 = EDGE_CURVE ( 'NONE', #15070, #20932, #13618, .T. ) ;
#11742 = EDGE_CURVE ( 'NONE', #16874, #18196, #17157, .T. ) ;
#11743 = ORIENTED_EDGE ( 'NONE', *, *, #10387, .T. ) ;
#11744 = CIRCLE ( 'NONE', #12787, 32.00000000000000000 ) ;
#11745 = ADVANCED_FACE ( 'NONE', ( #9273 ), #20892, .F. ) ;
#11746 = DIRECTION ( 'NONE',  ( -1.000000000000000000, 0.000000000000000000, 0.000000000000000000 ) ) ;
#11747 = LINE ( 'NONE', #149, #6008 ) ;
#11748 = AXIS2_PLACEMENT_3D ( 'NONE', #11161, #2773, #9496 ) ;
#11749 = ORIENTED_EDGE ( 'NONE', *, *, #13896, .T. ) ;
#11750 = CARTESIAN_POINT ( 'NONE',  ( -1.500000000000000000, -4.769696007084728073, 5.000000000000004441 ) ) ;
#11751 = EDGE_LOOP ( 'NONE', ( #4436, #4141, #6877, #21666 ) ) ;
#11752 = EDGE_CURVE ( 'NONE', #13981, #6087, #7323, .T. ) ;
#11753 = ORIENTED_EDGE ( 'NONE', *, *, #17606, .T. ) ;
#11754 = AXIS2_PLACEMENT_3D ( 'NONE', #6713, #387, #20281 ) ;
#11755 = DIRECTION ( 'NONE',  ( 1.000000000000000000, 0.000000000000000000, 0.000000000000000000 ) ) ;
#11756 = ORIENTED_EDGE ( 'NONE', *, *, #8371, .F. ) ;
#11757 = EDGE_LOOP ( 'NONE', ( #896, #12419, #16814, #4838 ) ) ;
#11758 = CARTESIAN_POINT ( 'NONE',  ( 10.00000000000000000, 36.60317927562682883, -76.78148674856727496 ) ) ;
#11759 = DIRECTION ( 'NONE',  ( 0.000000000000000000, 0.000000000000000000, -1.000000000000000000 ) ) ;
#11760 = AXIS2_PLACEMENT_3D ( 'NONE', #13301, #9977, #5017 ) ;
#11761 = ORIENTED_EDGE ( 'NONE', *, *, #6132, .T. ) ;
#11762 = ADVANCED_FACE ( 'NONE', ( #10621 ), #19129, .F. ) ;
#11763 = CARTESIAN_POINT ( 'NONE',  ( 10.00000000000000000, 57.53593069156372053, 72.42963261300981515 ) ) ;
#11764 = CARTESIAN_POINT ( 'NONE',  ( 0.000000000000000000, 5.479102470010468018, 87.82926298292115064 ) ) ;
#11765 = CYLINDRICAL_SURFACE ( 'NONE', #18905, 92.50100000000000477 ) ;
#11766 = CARTESIAN_POINT ( 'NONE',  ( 0.000000000000000000, 0.000000000000000000, 0.000000000000000000 ) ) ;
#11767 = CYLINDRICAL_SURFACE ( 'NONE', #12815, 44.99999999999999289 ) ;
#11768 = CARTESIAN_POINT ( 'NONE',  ( 10.00000000000000000, -8.925965667929485647, 92.06933331948778232 ) ) ;
#11769 = AXIS2_PLACEMENT_3D ( 'NONE', #2417, #12783, #4187 ) ;
#11770 = EDGE_CURVE ( 'NONE', #14184, #1184, #5160, .T. ) ;
#11771 = ORIENTED_EDGE ( 'NONE', *, *, #5859, .F. ) ;
#11772 = CARTESIAN_POINT ( 'NONE',  ( 0.000000000000000000, 0.000000000000000000, 0.000000000000000000 ) ) ;
#11773 = CIRCLE ( 'NONE', #17075, 92.50100000000000477 ) ;
#11774 = ADVANCED_FACE ( 'NONE', ( #20796 ), #2542, .F. ) ;
#11775 = FACE_OUTER_BOUND ( 'NONE', #5872, .T. ) ;
#11776 = ORIENTED_EDGE ( 'NONE', *, *, #8665, .T. ) ;
#11777 = AXIS2_PLACEMENT_3D ( 'NONE', #10886, #15962, #2493 ) ;
#11778 = DIRECTION ( 'NONE',  ( 0.000000000000000000, 0.000000000000000000, 1.000000000000000000 ) ) ;
#11779 = ORIENTED_EDGE ( 'NONE', *, *, #1103, .T. ) ;
#11780 = CARTESIAN_POINT ( 'NONE',  ( 0.000000000000000000, 0.000000000000000000, 0.000000000000000000 ) ) ;
#11781 = CARTESIAN_POINT ( 'NONE',  ( 10.00000000000000000, -15.32665449651985590, 91.22241316115413667 ) ) ;
#11782 = ORIENTED_EDGE ( 'NONE', *, *, #13082, .T. ) ;
#11783 = PLANE ( 'NONE',  #15911 ) ;
#11784 = EDGE_CURVE ( 'NONE', #1543, #11604, #4095, .T. ) ;
#11785 = CIRCLE ( 'NONE', #15294, 44.99999999999999289 ) ;
#11786 = ORIENTED_EDGE ( 'NONE', *, *, #11898, .T. ) ;
#11787 = ORIENTED_EDGE ( 'NONE', *, *, #9041, .T. ) ;
#11788 = VERTEX_POINT ( 'NONE', #14048 ) ;
#11789 = DIRECTION ( 'NONE',  ( 1.000000000000000000, 0.000000000000000000, 0.000000000000000000 ) ) ;
#11790 = EDGE_CURVE ( 'NONE', #16638, #5777, #17507, .T. ) ;
#11791 = VERTEX_POINT ( 'NONE', #10511 ) ;
#11792 = LINE ( 'NONE', #14168, #13371 ) ;
#11793 = AXIS2_PLACEMENT_3D ( 'NONE', #13875, #5491, #18974 ) ;
#11794 = DIRECTION ( 'NONE',  ( 0.000000000000000000, -0.2079116908177469081, -0.9781476007338082423 ) ) ;
#11795 = DIRECTION ( 'NONE',  ( 1.000000000000000000, 0.000000000000000000, 0.000000000000000000 ) ) ;
#11796 = LINE ( 'NONE', #4957, #5121 ) ;
#11797 = EDGE_CURVE ( 'NONE', #2646, #1841, #7973, .T. ) ;
#11798 = DIRECTION ( 'NONE',  ( 1.000000000000000000, 0.000000000000000000, 0.000000000000000000 ) ) ;
#11799 = AXIS2_PLACEMENT_3D ( 'NONE', #159, #1712, #5354 ) ;
#11800 = ADVANCED_FACE ( 'NONE', ( #891 ), #5548, .F. ) ;
#11801 = DIRECTION ( 'NONE',  ( 0.000000000000000000, -0.2756373558170063798, 0.9612616959383167847 ) ) ;
#11802 = DIRECTION ( 'NONE',  ( -1.000000000000000000, -0.000000000000000000, -0.000000000000000000 ) ) ;
#11803 = FACE_OUTER_BOUND ( 'NONE', #17687, .T. ) ;
#11804 = AXIS2_PLACEMENT_3D ( 'NONE', #490, #7233, #20498 ) ;
#11805 = EDGE_CURVE ( 'NONE', #966, #17521, #4804, .T. ) ;
#11806 = CARTESIAN_POINT ( 'NONE',  ( 10.00000000000000000, 80.18694381077148137, -28.37681241246572483 ) ) ;
#11807 = AXIS2_PLACEMENT_3D ( 'NONE', #2711, #14643, #4595 ) ;
#11808 = ORIENTED_EDGE ( 'NONE', *, *, #8035, .T. ) ;
#11809 = ORIENTED_EDGE ( 'NONE', *, *, #18912, .T. ) ;
#11810 = CARTESIAN_POINT ( 'NONE',  ( 1.199999999999992628, 0.000000000000000000, -6.728125000000023448 ) ) ;
#11811 = CIRCLE ( 'NONE', #16022, 6.500000000000000000 ) ;
#11812 = ORIENTED_EDGE ( 'NONE', *, *, #18685, .T. ) ;
#11813 = ORIENTED_EDGE ( 'NONE', *, *, #6361, .T. ) ;
#11814 = VERTEX_POINT ( 'NONE', #10729 ) ;
#11815 = CARTESIAN_POINT ( 'NONE',  ( 10.00000000000000000, -56.34908017029516714, -63.71789861856507997 ) ) ;
#11816 = ORIENTED_EDGE ( 'NONE', *, *, #16774, .T. ) ;
#11817 = DIRECTION ( 'NONE',  ( 1.000000000000000000, 0.000000000000000000, 0.000000000000000000 ) ) ;
#11818 = VECTOR ( 'NONE', #5654, 1000.000000000000000 ) ;
#11819 = CARTESIAN_POINT ( 'NONE',  ( 0.000000000000000000, 7.409634587003466777, -27.19958299168149907 ) ) ;
#11820 = AXIS2_PLACEMENT_3D ( 'NONE', #1511, #16221, #1079 ) ;
#11821 = EDGE_CURVE ( 'NONE', #6764, #4687, #10786, .T. ) ;
#11822 = DIRECTION ( 'NONE',  ( 1.000000000000000000, 0.000000000000000000, 0.000000000000000000 ) ) ;
#11823 = DIRECTION ( 'NONE',  ( 1.000000000000000000, 0.000000000000000000, 0.000000000000000000 ) ) ;
#11824 = DIRECTION ( 'NONE',  ( 0.000000000000000000, 0.000000000000000000, 1.000000000000000000 ) ) ;
#11825 = AXIS2_PLACEMENT_3D ( 'NONE', #5407, #8926, #21787 ) ;
#11826 = FACE_OUTER_BOUND ( 'NONE', #11672, .T. ) ;
#11827 = CARTESIAN_POINT ( 'NONE',  ( 0.000000000000000000, 0.000000000000000000, 0.000000000000000000 ) ) ;
#11828 = ORIENTED_EDGE ( 'NONE', *, *, #10387, .F. ) ;
#11829 = DIRECTION ( 'NONE',  ( 1.000000000000000000, 0.000000000000000000, 0.000000000000000000 ) ) ;
#11830 = CIRCLE ( 'NONE', #7953, 92.50100000000000477 ) ;
#11831 = ORIENTED_EDGE ( 'NONE', *, *, #2549, .F. ) ;
#11832 = CIRCLE ( 'NONE', #2663, 32.00000000000000000 ) ;
#11833 = VERTEX_POINT ( 'NONE', #9069 ) ;
#11834 = AXIS2_PLACEMENT_3D ( 'NONE', #9523, #16272, #9625 ) ;
#11835 = CARTESIAN_POINT ( 'NONE',  ( 0.000000000000000000, -28.15804365424196121, -1.358152127006266197 ) ) ;
#11836 = EDGE_LOOP ( 'NONE', ( #7444, #12752, #20510, #8869 ) ) ;
#11837 = DIRECTION ( 'NONE',  ( 1.000000000000000000, 0.000000000000000000, 0.000000000000000000 ) ) ;
#11838 = VERTEX_POINT ( 'NONE', #12279 ) ;
#11839 = EDGE_LOOP ( 'NONE', ( #20000, #8244, #15776, #1105 ) ) ;
#11840 = DIRECTION ( 'NONE',  ( 0.000000000000000000, 0.000000000000000000, 1.000000000000000000 ) ) ;
#11841 = ORIENTED_EDGE ( 'NONE', *, *, #9339, .F. ) ;
#11842 = EDGE_CURVE ( 'NONE', #17498, #14985, #19263, .T. ) ;
#11843 = CIRCLE ( 'NONE', #16415, 32.00000000000000000 ) ;
#11844 = LINE ( 'NONE', #1895, #5018 ) ;
#11845 = CIRCLE ( 'NONE', #1266, 12.00000000000000178 ) ;
#11846 = DIRECTION ( 'NONE',  ( 0.000000000000000000, 0.000000000000000000, 1.000000000000000000 ) ) ;
#11847 = CARTESIAN_POINT ( 'NONE',  ( 9.999999999999994671, 0.000000000000000000, 0.000000000000000000 ) ) ;
#11848 = AXIS2_PLACEMENT_3D ( 'NONE', #7917, #4706, #11445 ) ;
#11849 = DIRECTION ( 'NONE',  ( 0.000000000000000000, 0.7431448254773910245, 0.6691306063588617903 ) ) ;
#11850 = AXIS2_PLACEMENT_3D ( 'NONE', #20826, #20604, #7353 ) ;
#11851 = ADVANCED_FACE ( 'NONE', ( #685 ), #5766, .T. ) ;
#11852 = VECTOR ( 'NONE', #6268, 1000.000000000000000 ) ;
#11853 = DIRECTION ( 'NONE',  ( -1.000000000000000000, -0.000000000000000000, -0.000000000000000000 ) ) ;
#11854 = DIRECTION ( 'NONE',  ( 1.000000000000000000, 0.000000000000000000, 0.000000000000000000 ) ) ;
#11856 = VECTOR ( 'NONE', #6097, 1000.000000000000000 ) ;
#11855 = CARTESIAN_POINT ( 'NONE',  ( -1.200000000000006617, 8.434754829127421589E-16, 6.887500000000022382 ) ) ;
#11857 = ORIENTED_EDGE ( 'NONE', *, *, #3645, .F. ) ;
#11858 = FACE_OUTER_BOUND ( 'NONE', #13920, .T. ) ;
#11859 = CARTESIAN_POINT ( 'NONE',  ( 10.00000000000000000, 0.000000000000000000, 0.000000000000000000 ) ) ;
#11860 = ORIENTED_EDGE ( 'NONE', *, *, #8685, .F. ) ;
#11861 = CIRCLE ( 'NONE', #16088, 44.99999999999999289 ) ;
#11862 = DIRECTION ( 'NONE',  ( -1.000000000000000000, -0.000000000000000000, 0.000000000000000000 ) ) ;
#11863 = ORIENTED_EDGE ( 'NONE', *, *, #15293, .F. ) ;
#11864 = AXIS2_PLACEMENT_3D ( 'NONE', #18275, #12953, #1363 ) ;
#11865 = ORIENTED_EDGE ( 'NONE', *, *, #21072, .T. ) ;
#11866 = DIRECTION ( 'NONE',  ( -1.000000000000000000, 0.000000000000000000, 0.000000000000000000 ) ) ;
#11867 = VERTEX_POINT ( 'NONE', #15921 ) ;
#11868 = ADVANCED_FACE ( 'NONE', ( #21009 ), #4109, .F. ) ;
#11869 = VERTEX_POINT ( 'NONE', #778 ) ;
#11870 = DIRECTION ( 'NONE',  ( 1.000000000000000000, 0.000000000000000000, 0.000000000000000000 ) ) ;
#11871 = CARTESIAN_POINT ( 'NONE',  ( 10.00000000000000000, -21.98203405400967014, 17.64965094506536403 ) ) ;
#11872 = ORIENTED_EDGE ( 'NONE', *, *, #15035, .F. ) ;
#11873 = CARTESIAN_POINT ( 'NONE',  ( 10.00000000000000000, -21.65267340503189430, -89.93106657554454841 ) ) ;
#11874 = CARTESIAN_POINT ( 'NONE',  ( 0.000000000000000000, -29.47587714450981622, -82.91666097089152743 ) ) ;
#11875 = CARTESIAN_POINT ( 'NONE',  ( -10.00000000000000000, 0.000000000000000000, 0.000000000000000000 ) ) ;
#11876 = DIRECTION ( 'NONE',  ( 0.000000000000000000, 0.000000000000000000, 1.000000000000000000 ) ) ;
#11877 = FACE_OUTER_BOUND ( 'NONE', #14689, .T. ) ;
#11878 = CARTESIAN_POINT ( 'NONE',  ( 0.000000000000000000, 5.000000000000000000, 15.00000000000000000 ) ) ;
#11879 = VECTOR ( 'NONE', #8460, 1000.000000000000000 ) ;
#11880 = AXIS2_PLACEMENT_3D ( 'NONE', #18987, #17224, #3620 ) ;
#11881 = ORIENTED_EDGE ( 'NONE', *, *, #6, .F. ) ;
#11882 = DIRECTION ( 'NONE',  ( -1.000000000000000000, -0.000000000000000000, 0.000000000000000000 ) ) ;
#11883 = ADVANCED_FACE ( 'NONE', ( #19350 ), #4217, .T. ) ;
#11884 = CARTESIAN_POINT ( 'NONE',  ( 0.000000000000000000, -84.12297548659712731, -12.59025161327086906 ) ) ;
#11885 = ORIENTED_EDGE ( 'NONE', *, *, #18292, .T. ) ;
#11886 = DIRECTION ( 'NONE',  ( 0.000000000000000000, 0.000000000000000000, 1.000000000000000000 ) ) ;
#11887 = ORIENTED_EDGE ( 'NONE', *, *, #18758, .T. ) ;
#11888 = DIRECTION ( 'NONE',  ( -1.000000000000000000, -0.000000000000000000, 0.000000000000000000 ) ) ;
#11889 = CARTESIAN_POINT ( 'NONE',  ( 10.00000000000000000, 0.000000000000000000, 0.000000000000000000 ) ) ;
#11890 = ORIENTED_EDGE ( 'NONE', *, *, #17712, .T. ) ;
#11891 = VECTOR ( 'NONE', #6653, 1000.000000000000000 ) ;
#11893 = EDGE_CURVE ( 'NONE', #15626, #15275, #20669, .T. ) ;
#11892 = ORIENTED_EDGE ( 'NONE', *, *, #20845, .F. ) ;
#11894 = VERTEX_POINT ( 'NONE', #17919 ) ;
#11895 = EDGE_CURVE ( 'NONE', #19418, #21758, #9018, .T. ) ;
#11896 = CIRCLE ( 'NONE', #17547, 32.00000000000000000 ) ;
#11897 = ORIENTED_EDGE ( 'NONE', *, *, #12529, .T. ) ;
#11898 = EDGE_CURVE ( 'NONE', #11418, #3881, #12554, .T. ) ;
#11899 = FACE_OUTER_BOUND ( 'NONE', #4585, .T. ) ;
#11900 = VECTOR ( 'NONE', #17015, 1000.000000000000000 ) ;
#11901 = ORIENTED_EDGE ( 'NONE', *, *, #21081, .T. ) ;
#11902 = CARTESIAN_POINT ( 'NONE',  ( 10.00000000000000000, -27.26034713664092379, -7.182859710736426706 ) ) ;
#11903 = EDGE_CURVE ( 'NONE', #10412, #12425, #6209, .T. ) ;
#11904 = CARTESIAN_POINT ( 'NONE',  ( 10.00000000000000000, 0.000000000000000000, 0.000000000000000000 ) ) ;
#11905 = CARTESIAN_POINT ( 'NONE',  ( -140.0000507999999968, 4.000000000000000000, 0.000000000000000000 ) ) ;
#11906 = CARTESIAN_POINT ( 'NONE',  ( 10.00000000000000000, -65.64563793391792501, -54.09103124042881916 ) ) ;
#11907 = DIRECTION ( 'NONE',  ( -1.000000000000000000, 0.000000000000000000, 0.000000000000000000 ) ) ;
#11908 = EDGE_CURVE ( 'NONE', #15667, #5499, #1009, .T. ) ;
#11909 = CARTESIAN_POINT ( 'NONE',  ( 5.000000000000000000, -18.31866948046784671, 26.23788002993718393 ) ) ;
#11910 = CARTESIAN_POINT ( 'NONE',  ( 6.499999999999984901, 60.00000000000001421, 0.000000000000000000 ) ) ;
#11911 = DIRECTION ( 'NONE',  ( -1.000000000000000000, -0.000000000000000000, 0.000000000000000000 ) ) ;
#11912 = EDGE_CURVE ( 'NONE', #21782, #13331, #11050, .T. ) ;
#11913 = AXIS2_PLACEMENT_3D ( 'NONE', #14797, #16231, #4629 ) ;
#11914 = CARTESIAN_POINT ( 'NONE',  ( -140.0000507999999968, 6.123233995736766282E-16, 5.000000000000000000 ) ) ;
#11915 = AXIS2_PLACEMENT_3D ( 'NONE', #21742, #6625, #18339 ) ;
#11916 = EDGE_CURVE ( 'NONE', #12371, #14961, #2658, .T. ) ;
#11917 = CARTESIAN_POINT ( 'NONE',  ( 0.000000000000000000, 60.65655256511316651, -59.63197188857461128 ) ) ;
#11918 = EDGE_LOOP ( 'NONE', ( #1783, #1679, #20667, #7760 ) ) ;
#11919 = DIRECTION ( 'NONE',  ( 0.000000000000000000, 0.000000000000000000, 1.000000000000000000 ) ) ;
#11920 = ORIENTED_EDGE ( 'NONE', *, *, #15420, .F. ) ;
#11921 = DIRECTION ( 'NONE',  ( -1.000000000000000000, 0.000000000000000000, 0.000000000000000000 ) ) ;
#11922 = ADVANCED_FACE ( 'NONE', ( #19560 ), #4431, .F. ) ;
#11923 = ORIENTED_EDGE ( 'NONE', *, *, #15759, .F. ) ;
#11924 = ORIENTED_EDGE ( 'NONE', *, *, #4317, .F. ) ;
#11925 = ORIENTED_EDGE ( 'NONE', *, *, #248, .T. ) ;
#11926 = CARTESIAN_POINT ( 'NONE',  ( 10.00000000000000000, 72.53479564998846740, -44.42851404693280415 ) ) ;
#11927 = SHAPE_REPRESENTATION ( 'spur gear_iso_ISO - Spur gear 2M 30T 20PA 10FW ---S30B10H150L6.0S1', ( #15567 ), #19439 ) ;
#11928 = CIRCLE ( 'NONE', #2747, 44.99999999999999289 ) ;
#11929 = VECTOR ( 'NONE', #18837, 1000.000000000000000 ) ;
#11930 = ADVANCED_FACE ( 'NONE', ( #3957 ), #14451, .T. ) ;
#11931 = VERTEX_POINT ( 'NONE', #970 ) ;
#11932 = DIRECTION ( 'NONE',  ( 0.000000000000000000, 1.224646799147322392E-16, 1.000000000000000000 ) ) ;
#11933 = CIRCLE ( 'NONE', #2749, 11.99999999999999822 ) ;
#11934 = AXIS2_PLACEMENT_3D ( 'NONE', #17159, #7212, #2129 ) ;
#11935 = FACE_OUTER_BOUND ( 'NONE', #6342, .T. ) ;
#11936 = FACE_OUTER_BOUND ( 'NONE', #14470, .T. ) ;
#11937 = CYLINDRICAL_SURFACE ( 'NONE', #951, 11.99999999999999822 ) ;
#11938 = DIRECTION ( 'NONE',  ( -1.000000000000000000, 0.000000000000000000, 0.000000000000000000 ) ) ;
#11939 = LINE ( 'NONE', #8513, #9768 ) ;
#11940 = CARTESIAN_POINT ( 'NONE',  ( 10.00000000000000000, -43.18649929580243452, 73.28107340219401067 ) ) ;
#11941 = ORIENTED_EDGE ( 'NONE', *, *, #11312, .F. ) ;
#11942 = EDGE_CURVE ( 'NONE', #10332, #16155, #9143, .T. ) ;
#11943 = DIRECTION ( 'NONE',  ( 1.000000000000000000, 0.000000000000000000, 0.000000000000000000 ) ) ;
#11944 = AXIS2_PLACEMENT_3D ( 'NONE', #1328, #14808, #19999 ) ;
#11945 = CIRCLE ( 'NONE', #9470, 45.00000000000000711 ) ;
#11946 = ORIENTED_EDGE ( 'NONE', *, *, #3044, .F. ) ;
#11947 = VECTOR ( 'NONE', #12518, 1000.000000000000000 ) ;
#11948 = EDGE_CURVE ( 'NONE', #8942, #2674, #20335, .T. ) ;
#11949 = AXIS2_PLACEMENT_3D ( 'NONE', #15249, #11837, #13602 ) ;
#11950 = EDGE_CURVE ( 'NONE', #13666, #13798, #20758, .T. ) ;
#11951 = EDGE_LOOP ( 'NONE', ( #9404, #15496 ) ) ;
#11952 = DIRECTION ( 'NONE',  ( -1.000000000000000000, 0.000000000000000000, 0.000000000000000000 ) ) ;
#11953 = ORIENTED_EDGE ( 'NONE', *, *, #19892, .F. ) ;
#11954 = FACE_OUTER_BOUND ( 'NONE', #15037, .T. ) ;
#11955 = VERTEX_POINT ( 'NONE', #12777 ) ;
#11956 = ORIENTED_EDGE ( 'NONE', *, *, #15407, .F. ) ;
#11957 = CONTEXT_DEPENDENT_SHAPE_REPRESENTATION ( #6157, #13375 ) ;
#11958 = CARTESIAN_POINT ( 'NONE',  ( 10.00000000000000000, 0.000000000000000000, 0.000000000000000000 ) ) ;
#11959 = VERTEX_POINT ( 'NONE', #20861 ) ;
#11960 = CYLINDRICAL_SURFACE ( 'NONE', #9957, 92.50100000000000477 ) ;
#11961 = DIRECTION ( 'NONE',  ( 1.000000000000000000, 0.000000000000000000, 0.000000000000000000 ) ) ;
#11962 = DIRECTION ( 'NONE',  ( 1.000000000000000000, 0.000000000000000000, 0.000000000000000000 ) ) ;
#11963 = AXIS2_PLACEMENT_3D ( 'NONE', #9904, #16545, #8250 ) ;
#11964 = DIRECTION ( 'NONE',  ( -1.000000000000000000, 0.000000000000000000, 0.000000000000000000 ) ) ;
#11965 = CARTESIAN_POINT ( 'NONE',  ( 5.000000000000002665, -81.83745710415297481, 32.35167097270123548 ) ) ;
#11966 = CARTESIAN_POINT ( 'NONE',  ( 0.000000000000000000, 88.70892494636771630, -26.21376805916498043 ) ) ;
#11967 = DIRECTION ( 'NONE',  ( 0.000000000000000000, 0.000000000000000000, -1.000000000000000000 ) ) ;
#11968 = ORIENTED_EDGE ( 'NONE', *, *, #687, .F. ) ;
#11969 = DIRECTION ( 'NONE',  ( -1.000000000000000000, -0.000000000000000000, 0.000000000000000000 ) ) ;
#11970 = AXIS2_PLACEMENT_3D ( 'NONE', #18751, #16877, #20518 ) ;
#11971 = FACE_OUTER_BOUND ( 'NONE', #5913, .T. ) ;
#11972 = ORIENTED_EDGE ( 'NONE', *, *, #2046, .T. ) ;
#11973 = DIRECTION ( 'NONE',  ( -1.000000000000000000, 0.000000000000000000, 0.000000000000000000 ) ) ;
#11975 = AXIS2_PLACEMENT_3D ( 'NONE', #15112, #18665, #10352 ) ;
#11974 = PRODUCT ( 'center shaft', 'center shaft', '', ( #3220 ) ) ;
#11976 = ORIENTED_EDGE ( 'NONE', *, *, #13363, .F. ) ;
#11977 = ORIENTED_EDGE ( 'NONE', *, *, #17217, .T. ) ;
#11978 = CARTESIAN_POINT ( 'NONE',  ( 10.00000000000000000, 24.73395913766463750, 12.01774797440586084 ) ) ;
#11979 = ORIENTED_EDGE ( 'NONE', *, *, #10150, .T. ) ;
#11980 = ORIENTED_EDGE ( 'NONE', *, *, #12600, .T. ) ;
#11981 = FACE_OUTER_BOUND ( 'NONE', #2997, .T. ) ;
#11982 = CARTESIAN_POINT ( 'NONE',  ( 0.000000000000000000, 0.000000000000000000, 0.000000000000000000 ) ) ;
#11983 = CARTESIAN_POINT ( 'NONE',  ( 0.000000000000000000, -19.85071254963763465, -20.01672328094552356 ) ) ;
#11984 = FACE_OUTER_BOUND ( 'NONE', #17500, .T. ) ;
#11985 = DIRECTION ( 'NONE',  ( -1.000000000000000000, -0.000000000000000000, -0.000000000000000000 ) ) ;
#11986 = CARTESIAN_POINT ( 'NONE',  ( -90.00000000000000000, 6.873330160214519262E-16, 5.612499999999999822 ) ) ;
#11987 = DIRECTION ( 'NONE',  ( -1.000000000000000000, 0.000000000000000000, 0.000000000000000000 ) ) ;
#11988 = FACE_OUTER_BOUND ( 'NONE', #5701, .T. ) ;
#11989 = AXIS2_PLACEMENT_3D ( 'NONE', #8330, #20376, #1701 ) ;
#11990 = ORIENTED_EDGE ( 'NONE', *, *, #7093, .T. ) ;
#11991 = AXIS2_PLACEMENT_3D ( 'NONE', #8352, #15082, #8566 ) ;
#11992 = DIRECTION ( 'NONE',  ( 0.000000000000000000, 0.000000000000000000, 1.000000000000000000 ) ) ;
#11993 = DIRECTION ( 'NONE',  ( 0.000000000000000000, 0.000000000000000000, 1.000000000000000000 ) ) ;
#11994 = ADVANCED_FACE ( 'NONE', ( #20970 ), #2623, .F. ) ;
#11995 = ORIENTED_EDGE ( 'NONE', *, *, #15930, .F. ) ;
#11996 = CARTESIAN_POINT ( 'NONE',  ( 10.00000000000000000, 92.49798535263882115, 0.7467976319023850174 ) ) ;
#11997 = ORIENTED_EDGE ( 'NONE', *, *, #3213, .F. ) ;
#11998 = CYLINDRICAL_SURFACE ( 'NONE', #13394, 44.99999999999999289 ) ;
#11999 = DIRECTION ( 'NONE',  ( 0.000000000000000000, 0.000000000000000000, -1.000000000000000000 ) ) ;
#12000 = ORIENTED_EDGE ( 'NONE', *, *, #19059, .T. ) ;
#12001 = EDGE_CURVE ( 'NONE', #5809, #15140, #10081, .T. ) ;
#12002 =( NAMED_UNIT ( * ) PLANE_ANGLE_UNIT ( ) SI_UNIT ( $, .RADIAN. ) );
#12003 = VERTEX_POINT ( 'NONE', #5627 ) ;
#12004 = ORIENTED_EDGE ( 'NONE', *, *, #17323, .F. ) ;
#12005 = ORIENTED_EDGE ( 'NONE', *, *, #11912, .T. ) ;
#12006 = CIRCLE ( 'NONE', #18012, 11.99999999999999822 ) ;
#12007 = CARTESIAN_POINT ( 'NONE',  ( -120.0000000000000000, 1.469576158976823671E-14, 0.000000000000000000 ) ) ;
#12008 = VERTEX_POINT ( 'NONE', #10799 ) ;
#12009 = CARTESIAN_POINT ( 'NONE',  ( 10.00000000000000000, 1.592605004253184964, -28.14575649959892445 ) ) ;
#12010 = LINE ( 'NONE', #81, #14253 ) ;
#12011 = CARTESIAN_POINT ( 'NONE',  ( 0.000000000000000000, -8.925965667928249303, -92.06933331948791022 ) ) ;
#12012 = CARTESIAN_POINT ( 'NONE',  ( 10.00000000000000000, 65.64563793391906188, -54.09103124042745492 ) ) ;
#12013 = CARTESIAN_POINT ( 'NONE',  ( 0.000000000000000000, 46.07110168784925008, -74.97635353408335845 ) ) ;
#12014 = DIRECTION ( 'NONE',  ( -1.000000000000000000, -0.000000000000000000, -0.000000000000000000 ) ) ;
#12015 = DIRECTION ( 'NONE',  ( 0.000000000000000000, 0.000000000000000000, -1.000000000000000000 ) ) ;
#12016 = DIRECTION ( 'NONE',  ( 0.000000000000000000, 0.000000000000000000, 1.000000000000000000 ) ) ;
#12017 = VERTEX_POINT ( 'NONE', #5951 ) ;
#12018 = DIRECTION ( 'NONE',  ( -1.000000000000000000, 0.000000000000000000, 0.000000000000000000 ) ) ;
#12019 = DIRECTION ( 'NONE',  ( 0.000000000000000000, 0.000000000000000000, 1.000000000000000000 ) ) ;
#12020 = EDGE_CURVE ( 'NONE', #1889, #21386, #5870, .T. ) ;
#12021 = EDGE_CURVE ( 'NONE', #13109, #1355, #914, .T. ) ;
#12022 = EDGE_CURVE ( 'NONE', #20543, #15549, #12357, .T. ) ;
#12023 = AXIS2_PLACEMENT_3D ( 'NONE', #13269, #18145, #20237 ) ;
#12024 = CYLINDRICAL_SURFACE ( 'NONE', #21423, 92.50100000000000477 ) ;
#12025 = ORIENTED_EDGE ( 'NONE', *, *, #12288, .T. ) ;
#12026 = EDGE_CURVE ( 'NONE', #7417, #1350, #1982, .T. ) ;
#12027 = LINE ( 'NONE', #20106, #15475 ) ;
#12028 = ORIENTED_EDGE ( 'NONE', *, *, #11271, .T. ) ;
#12029 = CARTESIAN_POINT ( 'NONE',  ( 0.000000000000000000, -41.87002153499162915, 74.04114219178029543 ) ) ;
#12030 = ORIENTED_EDGE ( 'NONE', *, *, #2050, .T. ) ;
#12031 = ORIENTED_EDGE ( 'NONE', *, *, #5792, .T. ) ;
#12032 = VERTEX_POINT ( 'NONE', #17339 ) ;
#12033 = EDGE_CURVE ( 'NONE', #12565, #14140, #12568, .T. ) ;
#12034 = CARTESIAN_POINT ( 'NONE',  ( 0.000000000000000000, -9.646732466564730046, -84.51112348751858860 ) ) ;
#12035 = EDGE_LOOP ( 'NONE', ( #21429, #458 ) ) ;
#12036 = CARTESIAN_POINT ( 'NONE',  ( 0.000000000000000000, 0.000000000000000000, 0.000000000000000000 ) ) ;
#12037 = CARTESIAN_POINT ( 'NONE',  ( -1.500000000000000000, 15.00000000000000000, 4.769696007084728073 ) ) ;
#12038 = PRESENTATION_LAYER_ASSIGNMENT (  '', '', ( #21560 ) ) ;
#12039 =( LENGTH_UNIT ( ) NAMED_UNIT ( * ) SI_UNIT ( .MILLI., .METRE. ) );
#12040 = ADVANCED_FACE ( 'NONE', ( #9031 ), #15778, .F. ) ;
#12041 = CARTESIAN_POINT ( 'NONE',  ( 10.00000000000000000, 0.000000000000000000, 0.000000000000000000 ) ) ;
#12042 = CARTESIAN_POINT ( 'NONE',  ( 0.000000000000000000, -85.54350296776125617, 20.64725405482824883 ) ) ;
#12043 = FACE_OUTER_BOUND ( 'NONE', #219, .T. ) ;
#12044 = DIRECTION ( 'NONE',  ( 0.000000000000000000, 0.6427876096865353661, 0.7660444431189814551 ) ) ;
#12045 = DIRECTION ( 'NONE',  ( 0.000000000000000000, 1.224646799147368738E-16, 1.000000000000000000 ) ) ;
#12046 = ORIENTED_EDGE ( 'NONE', *, *, #4468, .F. ) ;
#12047 = CARTESIAN_POINT ( 'NONE',  ( 10.00000000000000000, 0.000000000000000000, 0.000000000000000000 ) ) ;
#12048 = EDGE_CURVE ( 'NONE', #8158, #16874, #3746, .T. ) ;
#12049 = ORIENTED_EDGE ( 'NONE', *, *, #20721, .F. ) ;
#12050 = VERTEX_POINT ( 'NONE', #15988 ) ;
#12051 = DIRECTION ( 'NONE',  ( 0.000000000000000000, 0.000000000000000000, 1.000000000000000000 ) ) ;
#12052 = ORIENTED_EDGE ( 'NONE', *, *, #9740, .T. ) ;
#12053 = ORIENTED_EDGE ( 'NONE', *, *, #8124, .T. ) ;
#12054 = EDGE_CURVE ( 'NONE', #16691, #1024, #855, .T. ) ;
#12055 = DIRECTION ( 'NONE',  ( -1.000000000000000000, 0.000000000000000000, 0.000000000000000000 ) ) ;
#12056 = ORIENTED_EDGE ( 'NONE', *, *, #12465, .T. ) ;
#12057 = ADVANCED_FACE ( 'NONE', ( #21084 ), #19419, .F. ) ;
#12058 = CARTESIAN_POINT ( 'NONE',  ( 10.00000000000000000, 0.000000000000000000, 0.000000000000000000 ) ) ;
#12059 = CARTESIAN_POINT ( 'NONE',  ( 0.000000000000000000, 65.83713140174806711, -58.39068529131128571 ) ) ;
#12060 = DIRECTION ( 'NONE',  ( 0.000000000000000000, 0.000000000000000000, -1.000000000000000000 ) ) ;
#12061 = LINE ( 'NONE', #20573, #1980 ) ;
#12062 = EDGE_CURVE ( 'NONE', #16531, #5649, #9354, .T. ) ;
#12063 = EDGE_CURVE ( 'NONE', #10683, #4886, #525, .T. ) ;
#12064 = DIRECTION ( 'NONE',  ( -1.000000000000000000, 0.000000000000000000, 0.000000000000000000 ) ) ;
#12065 = FACE_OUTER_BOUND ( 'NONE', #9650, .T. ) ;
#12066 = DIRECTION ( 'NONE',  ( 0.000000000000000000, -0.06975647374413235235, 0.9975640502598237536 ) ) ;
#12067 = VERTEX_POINT ( 'NONE', #9676 ) ;
#12068 = ADVANCED_FACE ( 'NONE', ( #17999 ), #2951, .T. ) ;
#12069 = DIRECTION ( 'NONE',  ( -1.000000000000000000, 0.000000000000000000, -0.000000000000000000 ) ) ;
#12070 = APPLICATION_CONTEXT ( 'automotive_design' ) ;
#12071 = DIRECTION ( 'NONE',  ( -1.000000000000000000, -0.000000000000000000, 0.000000000000000000 ) ) ;
#12072 = ORIENTED_EDGE ( 'NONE', *, *, #1722, .T. ) ;
#12073 = DIRECTION ( 'NONE',  ( 0.000000000000000000, 0.000000000000000000, 1.000000000000000000 ) ) ;
#12074 = ORIENTED_EDGE ( 'NONE', *, *, #9628, .F. ) ;
#12075 = ORIENTED_EDGE ( 'NONE', *, *, #5519, .F. ) ;
#12076 = CARTESIAN_POINT ( 'NONE',  ( 10.00000000000000000, -62.44821182181136976, 68.23969402963483333 ) ) ;
#12077 = VECTOR ( 'NONE', #13607, 1000.000000000000000 ) ;
#12078 = EDGE_LOOP ( 'NONE', ( #15507, #15924, #8473, #6938 ) ) ;
#12079 = ORIENTED_EDGE ( 'NONE', *, *, #20367, .F. ) ;
#12080 = FACE_OUTER_BOUND ( 'NONE', #1210, .T. ) ;
#12081 = DIRECTION ( 'NONE',  ( -1.000000000000000000, 0.000000000000000000, 0.000000000000000000 ) ) ;
#12082 = VECTOR ( 'NONE', #8608, 1000.000000000000000 ) ;
#12083 = FACE_OUTER_BOUND ( 'NONE', #8151, .T. ) ;
#12084 = DIRECTION ( 'NONE',  ( 1.000000000000000000, -0.000000000000000000, -0.000000000000000000 ) ) ;
#12085 = CARTESIAN_POINT ( 'NONE',  ( 0.000000000000000000, 21.65267340503369198, -89.93106657554412209 ) ) ;
#12086 = DIRECTION ( 'NONE',  ( 1.000000000000000000, 0.000000000000000000, 0.000000000000000000 ) ) ;
#12087 = AXIS2_PLACEMENT_3D ( 'NONE', #3077, #11802, #21536 ) ;
#12088 = DIRECTION ( 'NONE',  ( 1.000000000000000000, 0.000000000000000000, -0.000000000000000000 ) ) ;
#12089 = FACE_OUTER_BOUND ( 'NONE', #1386, .T. ) ;
#12090 = ORIENTED_EDGE ( 'NONE', *, *, #8241, .F. ) ;
#12091 = DIRECTION ( 'NONE',  ( 0.000000000000000000, -0.7431448254773861395, -0.6691306063588672304 ) ) ;
#12092 = CIRCLE ( 'NONE', #18805, 1.100000000000003642 ) ;
#12093 = CARTESIAN_POINT ( 'NONE',  ( 10.00000000000000000, -78.83848282823873888, -48.38314403117582430 ) ) ;
#12094 = VERTEX_POINT ( 'NONE', #1186 ) ;
#12095 = CYLINDRICAL_SURFACE ( 'NONE', #9416, 92.50100000000000477 ) ;
#12096 = ORIENTED_EDGE ( 'NONE', *, *, #4782, .F. ) ;
#12097 = CIRCLE ( 'NONE', #4657, 92.50100000000001899 ) ;
#12098 = CARTESIAN_POINT ( 'NONE',  ( 10.00000000000000000, 71.33759994382042180, -58.88447872958914786 ) ) ;
#12099 = CARTESIAN_POINT ( 'NONE',  ( 8.899999999999991473, 0.000000000000000000, 0.000000000000000000 ) ) ;
#12100 = ORIENTED_EDGE ( 'NONE', *, *, #2328, .T. ) ;
#12101 = CIRCLE ( 'NONE', #19514, 88.00000000000000000 ) ;
#12102 = DIRECTION ( 'NONE',  ( 0.000000000000000000, -0.2079116908177664480, 0.9781476007338041345 ) ) ;
#12103 = ORIENTED_EDGE ( 'NONE', *, *, #18393, .F. ) ;
#12104 = ORIENTED_EDGE ( 'NONE', *, *, #13953, .F. ) ;
#12105 = ORIENTED_EDGE ( 'NONE', *, *, #3418, .F. ) ;
#12106 = FACE_OUTER_BOUND ( 'NONE', #15854, .T. ) ;
#12107 = EDGE_CURVE ( 'NONE', #3061, #3876, #11138, .T. ) ;
#12108 = ORIENTED_EDGE ( 'NONE', *, *, #13060, .T. ) ;
#12109 = DIRECTION ( 'NONE',  ( 0.000000000000000000, 0.000000000000000000, 1.000000000000000000 ) ) ;
#12110 = DIRECTION ( 'NONE',  ( 1.000000000000000000, 0.000000000000000000, 0.000000000000000000 ) ) ;
#12111 = CARTESIAN_POINT ( 'NONE',  ( 0.000000000000000000, 47.19205848891765243, 74.27590198428138990 ) ) ;
#12112 = EDGE_CURVE ( 'NONE', #1041, #4641, #8156, .T. ) ;
#12113 = CARTESIAN_POINT ( 'NONE',  ( 0.000000000000000000, 0.6609040254611577847, 87.99751818016873983 ) ) ;
#12114 = LINE ( 'NONE', #13671, #9636 ) ;
#12115 = DIRECTION ( 'NONE',  ( -1.000000000000000000, 0.000000000000000000, 0.000000000000000000 ) ) ;
#12116 = CARTESIAN_POINT ( 'NONE',  ( -10.00000000000000000, 0.000000000000000000, 0.000000000000000000 ) ) ;
#12117 = CARTESIAN_POINT ( 'NONE',  ( 0.000000000000000000, 71.72924546249947753, 45.71766382684695884 ) ) ;
#12118 = ORIENTED_EDGE ( 'NONE', *, *, #19569, .F. ) ;
#12119 = ADVANCED_FACE ( 'NONE', ( #9792 ), #4511, .F. ) ;
#12120 = VECTOR ( 'NONE', #16267, 1000.000000000000000 ) ;
#12121 = CYLINDRICAL_SURFACE ( 'NONE', #14804, 44.99999999999999289 ) ;
#12122 = TOROIDAL_SURFACE ( 'NONE', #4711, 105.0992000000000104, 0.2042000000000007420 ) ;
#12123 = DIRECTION ( 'NONE',  ( 1.000000000000000000, 0.000000000000000000, 0.000000000000000000 ) ) ;
#12124 = CARTESIAN_POINT ( 'NONE',  ( 0.000000000000000000, 6.797690662955227836, 87.73705831432218361 ) ) ;
#12125 = ORIENTED_EDGE ( 'NONE', *, *, #6788, .T. ) ;
#12126 = CIRCLE ( 'NONE', #2251, 44.99999999999999289 ) ;
#12127 = DIRECTION ( 'NONE',  ( 1.000000000000000000, 0.000000000000000000, 0.000000000000000000 ) ) ;
#12128 = ORIENTED_EDGE ( 'NONE', *, *, #9578, .T. ) ;
#12129 = CARTESIAN_POINT ( 'NONE',  ( 0.000000000000000000, 70.37753541436022431, -60.02863908169561569 ) ) ;
#12130 = VERTEX_POINT ( 'NONE', #18095 ) ;
#12131 = AXIS2_PLACEMENT_3D ( 'NONE', #21683, #6573, #20147 ) ;
#12132 = ORIENTED_EDGE ( 'NONE', *, *, #18283, .T. ) ;
#12133 = AXIS2_PLACEMENT_3D ( 'NONE', #12540, #20617, #10564 ) ;
#12134 = ORIENTED_EDGE ( 'NONE', *, *, #3671, .F. ) ;
#12135 = DIRECTION ( 'NONE',  ( 1.000000000000000000, 0.000000000000000000, 0.000000000000000000 ) ) ;
#12136 = CARTESIAN_POINT ( 'NONE',  ( 10.00000000000000000, 0.000000000000000000, 0.000000000000000000 ) ) ;
#12137 = CARTESIAN_POINT ( 'NONE',  ( 0.000000000000000000, -10.41137886060045048, -91.91321010181856366 ) ) ;
#12138 = EDGE_CURVE ( 'NONE', #13033, #2027, #6292, .T. ) ;
#12139 = ADVANCED_FACE ( 'NONE', ( #14992 ), #8048, .F. ) ;
#12140 = FACE_OUTER_BOUND ( 'NONE', #9232, .T. ) ;
#12141 = CIRCLE ( 'NONE', #1907, 88.00000000000000000 ) ;
#12142 = CYLINDRICAL_SURFACE ( 'NONE', #2211, 92.50100000000000477 ) ;
#12143 = CARTESIAN_POINT ( 'NONE',  ( -90.00000000000000000, 1.409568465818603827E-14, 115.1000000000000227 ) ) ;
#12144 = DIRECTION ( 'NONE',  ( 0.000000000000000000, -0.000000000000000000, -1.000000000000000000 ) ) ;
#12145 = DIRECTION ( 'NONE',  ( -1.000000000000000000, 0.000000000000000000, -0.000000000000000000 ) ) ;
#12146 = CARTESIAN_POINT ( 'NONE',  ( 10.00000000000000000, 23.57863763525720202, 15.45211464167672588 ) ) ;
#12147 = VECTOR ( 'NONE', #17644, 1000.000000000000000 ) ;
#12148 = ORIENTED_EDGE ( 'NONE', *, *, #10137, .F. ) ;
#12149 = AXIS2_PLACEMENT_3D ( 'NONE', #19806, #4336, #9405 ) ;
#12150 = FACE_OUTER_BOUND ( 'NONE', #15950, .T. ) ;
#12151 = EDGE_CURVE ( 'NONE', #2087, #17425, #14886, .T. ) ;
#12152 = ORIENTED_EDGE ( 'NONE', *, *, #10439, .F. ) ;
#12153 = EDGE_LOOP ( 'NONE', ( #18033, #19876, #6980, #13184 ) ) ;
#12154 = EDGE_CURVE ( 'NONE', #2139, #17111, #21527, .T. ) ;
#12155 = DIRECTION ( 'NONE',  ( -1.000000000000000000, -0.000000000000000000, -0.000000000000000000 ) ) ;
#12156 = VECTOR ( 'NONE', #8837, 1000.000000000000000 ) ;
#12157 = ORIENTED_EDGE ( 'NONE', *, *, #16389, .T. ) ;
#12158 = VERTEX_POINT ( 'NONE', #13113 ) ;
#12159 = AXIS2_PLACEMENT_3D ( 'NONE', #7818, #19855, #18212 ) ;
#12160 = VECTOR ( 'NONE', #706, 1000.000000000000000 ) ;
#12161 = CARTESIAN_POINT ( 'NONE',  ( 10.00000000000000000, 0.000000000000000000, 0.000000000000000000 ) ) ;
#12162 = EDGE_CURVE ( 'NONE', #374, #12679, #14986, .T. ) ;
#12163 = VERTEX_POINT ( 'NONE', #3067 ) ;
#12164 = EDGE_CURVE ( 'NONE', #3424, #12008, #15694, .T. ) ;
#12165 = ADVANCED_FACE ( 'NONE', ( #12897 ), #1418, .F. ) ;
#12166 = CIRCLE ( 'NONE', #11825, 27.49900000000000233 ) ;
#12167 = DIRECTION ( 'NONE',  ( -1.000000000000000000, -0.000000000000000000, -0.000000000000000000 ) ) ;
#12168 = EDGE_CURVE ( 'NONE', #14884, #12349, #580, .T. ) ;
#12169 = FACE_OUTER_BOUND ( 'NONE', #5012, .T. ) ;
#12170 = CARTESIAN_POINT ( 'NONE',  ( 10.00000000000000000, 0.000000000000000000, 0.000000000000000000 ) ) ;
#12171 = DIRECTION ( 'NONE',  ( 0.000000000000000000, 0.000000000000000000, 1.000000000000000000 ) ) ;
#12172 = DIRECTION ( 'NONE',  ( -1.000000000000000000, 0.000000000000000000, 0.000000000000000000 ) ) ;
#12173 = FACE_OUTER_BOUND ( 'NONE', #13957, .T. ) ;
#12174 = CARTESIAN_POINT ( 'NONE',  ( 10.00000000000000000, 92.22057093985038989, -7.197311757039552838 ) ) ;
#12175 = ORIENTED_EDGE ( 'NONE', *, *, #21463, .F. ) ;
#12176 = AXIS2_PLACEMENT_3D ( 'NONE', #15968, #835, #21061 ) ;
#12177 = EDGE_CURVE ( 'NONE', #5209, #2646, #9909, .T. ) ;
#12178 = AXIS2_PLACEMENT_3D ( 'NONE', #10072, #18712, #13492 ) ;
#12179 = EDGE_CURVE ( 'NONE', #9724, #15532, #1581, .T. ) ;
#12180 = AXIS2_PLACEMENT_3D ( 'NONE', #6833, #3831, #12223 ) ;
#12181 = DIRECTION ( 'NONE',  ( 1.000000000000000000, 0.000000000000000000, 0.000000000000000000 ) ) ;
#12182 = EDGE_CURVE ( 'NONE', #3222, #3530, #21295, .T. ) ;
#12183 = DIRECTION ( 'NONE',  ( 1.000000000000000000, -0.000000000000000000, -0.000000000000000000 ) ) ;
#12184 = VERTEX_POINT ( 'NONE', #16318 ) ;
#12185 = CIRCLE ( 'NONE', #4085, 92.50100000000000477 ) ;
#12186 = CARTESIAN_POINT ( 'NONE',  ( 10.00000000000000000, 0.000000000000000000, 0.000000000000000000 ) ) ;
#12187 = ORIENTED_EDGE ( 'NONE', *, *, #1472, .T. ) ;
#12188 = EDGE_CURVE ( 'NONE', #3466, #20932, #18583, .T. ) ;
#12189 = PRESENTATION_STYLE_ASSIGNMENT (( #17171 ) ) ;
#12190 = DIRECTION ( 'NONE',  ( -1.000000000000000000, 0.000000000000000000, 0.000000000000000000 ) ) ;
#12191 = ORIENTED_EDGE ( 'NONE', *, *, #3645, .T. ) ;
#12192 = AXIS2_PLACEMENT_3D ( 'NONE', #2547, #13047, #16258 ) ;
#12193 = ORIENTED_EDGE ( 'NONE', *, *, #20575, .T. ) ;
#12194 = DIRECTION ( 'NONE',  ( 0.000000000000000000, 0.000000000000000000, 1.000000000000000000 ) ) ;
#12195 = CYLINDRICAL_SURFACE ( 'NONE', #1486, 88.00000000000000000 ) ;
#12196 = AXIS2_PLACEMENT_3D ( 'NONE', #2461, #21020, #7439 ) ;
#12197 = AXIS2_PLACEMENT_3D ( 'NONE', #5337, #10400, #7106 ) ;
#12198 = EDGE_CURVE ( 'NONE', #19416, #7568, #6510, .T. ) ;
#12199 = DIRECTION ( 'NONE',  ( 0.000000000000000000, 0.000000000000000000, 1.000000000000000000 ) ) ;
#12200 = CARTESIAN_POINT ( 'NONE',  ( 10.00000000000000000, -89.12061559554348378, 24.77803214283513356 ) ) ;
#12201 = CYLINDRICAL_SURFACE ( 'NONE', #18203, 88.00000000000000000 ) ;
#12202 = FACE_OUTER_BOUND ( 'NONE', #16612, .T. ) ;
#12203 = LINE ( 'NONE', #10221, #13880 ) ;
#12204 = CARTESIAN_POINT ( 'NONE',  ( 10.00000000000000888, 1.462840601581513680E-14, 118.9000000000000199 ) ) ;
#12205 = EDGE_LOOP ( 'NONE', ( #6471, #16486, #721, #9674 ) ) ;
#12206 = CARTESIAN_POINT ( 'NONE',  ( 0.000000000000000000, -86.66425444033897918, -32.33793443156484670 ) ) ;
#12207 = ORIENTED_EDGE ( 'NONE', *, *, #17292, .F. ) ;
#12208 = AXIS2_PLACEMENT_3D ( 'NONE', #12047, #446, #13708 ) ;
#12209 = EDGE_CURVE ( 'NONE', #5375, #7808, #13928, .T. ) ;
#12210 = PRESENTATION_LAYER_ASSIGNMENT (  '', '', ( #17869 ) ) ;
#12211 = CARTESIAN_POINT ( 'NONE',  ( 0.000000000000000000, -40.72878876293093242, -78.00747250042492453 ) ) ;
#12212 = AXIS2_PLACEMENT_3D ( 'NONE', #21220, #9914, #11465 ) ;
#12213 = EDGE_LOOP ( 'NONE', ( #178, #16189, #6012, #15536 ) ) ;
#12214 = DIRECTION ( 'NONE',  ( 0.000000000000000000, 0.000000000000000000, 1.000000000000000000 ) ) ;
#12215 = DIRECTION ( 'NONE',  ( 1.000000000000000000, 0.000000000000000000, 0.000000000000000000 ) ) ;
#12216 = EDGE_LOOP ( 'NONE', ( #19021, #15243, #2991, #19546 ) ) ;
#12217 = EDGE_CURVE ( 'NONE', #21597, #13328, #3347, .T. ) ;
#12218 = ORIENTED_EDGE ( 'NONE', *, *, #10712, .F. ) ;
#12219 = EDGE_LOOP ( 'NONE', ( #20059, #16429, #18067, #5213 ) ) ;
#12220 = ORIENTED_EDGE ( 'NONE', *, *, #21733, .T. ) ;
#12221 = CARTESIAN_POINT ( 'NONE',  ( 150.0000507999999968, 4.000000000000000000, -1.000000000000000000 ) ) ;
#12222 = ORIENTED_EDGE ( 'NONE', *, *, #16251, .F. ) ;
#12223 = DIRECTION ( 'NONE',  ( 0.000000000000000000, 0.7880107536067190166, 0.6156614753256620665 ) ) ;
#12224 = DIRECTION ( 'NONE',  ( -1.000000000000000000, 0.000000000000000000, 0.000000000000000000 ) ) ;
#12225 = CIRCLE ( 'NONE', #11880, 11.99999999999999822 ) ;
#12226 = DIRECTION ( 'NONE',  ( 0.000000000000000000, 0.000000000000000000, 1.000000000000000000 ) ) ;
#12227 = CARTESIAN_POINT ( 'NONE',  ( 5.000000000000002665, -83.89484365856893078, -26.56417150043033359 ) ) ;
#12228 = AXIS2_PLACEMENT_3D ( 'NONE', #2223, #20891, #21119 ) ;
#12229 = CARTESIAN_POINT ( 'NONE',  ( 10.00000000000000000, 0.000000000000000000, 0.000000000000000000 ) ) ;
#12230 = DIRECTION ( 'NONE',  ( -1.000000000000000000, 0.000000000000000000, 0.000000000000000000 ) ) ;
#12231 = ORIENTED_EDGE ( 'NONE', *, *, #118, .F. ) ;
#12232 = CARTESIAN_POINT ( 'NONE',  ( 5.000000000000000000, 64.95266917914317162, 59.37298010462993858 ) ) ;
#12233 = EDGE_CURVE ( 'NONE', #4620, #16625, #1639, .T. ) ;
#12234 = DIRECTION ( 'NONE',  ( 0.000000000000000000, 0.000000000000000000, -1.000000000000000000 ) ) ;
#12235 = VERTEX_POINT ( 'NONE', #8265 ) ;
#12236 = CIRCLE ( 'NONE', #5888, 44.99999999999999289 ) ;
#12237 = LINE ( 'NONE', #9023, #10897 ) ;
#12238 = CIRCLE ( 'NONE', #4488, 44.99999999999999289 ) ;
#12239 = ORIENTED_EDGE ( 'NONE', *, *, #12945, .F. ) ;
#12240 = DIRECTION ( 'NONE',  ( -1.000000000000000000, -0.000000000000000000, -0.000000000000000000 ) ) ;
#12241 = AXIS2_PLACEMENT_3D ( 'NONE', #8612, #18895, #13586 ) ;
#12242 = ORIENTED_EDGE ( 'NONE', *, *, #2702, .F. ) ;
#12243 = ORIENTED_EDGE ( 'NONE', *, *, #919, .T. ) ;
#12244 = ORIENTED_EDGE ( 'NONE', *, *, #11524, .F. ) ;
#12245 = CYLINDRICAL_SURFACE ( 'NONE', #661, 115.1000000000000227 ) ;
#12246 = LINE ( 'NONE', #7171, #15333 ) ;
#12247 = DIRECTION ( 'NONE',  ( -1.000000000000000000, -0.000000000000000000, 0.000000000000000000 ) ) ;
#12248 = DIRECTION ( 'NONE',  ( -0.000000000000000000, -1.000000000000000000, -0.000000000000000000 ) ) ;
#12249 = PRODUCT_DEFINITION_CONTEXT ( 'detailed design', #14469, 'design' ) ;
#12250 = DIRECTION ( 'NONE',  ( -1.000000000000000000, -0.000000000000000000, -0.000000000000000000 ) ) ;
#12251 = AXIS2_PLACEMENT_3D ( 'NONE', #7244, #6820, #8472 ) ;
#12252 = CARTESIAN_POINT ( 'NONE',  ( 10.00000000000000000, 0.000000000000000000, 0.000000000000000000 ) ) ;
#12253 = CARTESIAN_POINT ( 'NONE',  ( 5.000000000000002665, 12.90135963484197212, -87.04915231966633371 ) ) ;
#12254 = CIRCLE ( 'NONE', #21436, 5.100000000000000533 ) ;
#12255 = CYLINDRICAL_SURFACE ( 'NONE', #15421, 11.99999999999999645 ) ;
#12256 = CARTESIAN_POINT ( 'NONE',  ( 10.00000000000000000, -30.24235385705231138, -10.45944707835137955 ) ) ;
#12257 = ORIENTED_EDGE ( 'NONE', *, *, #9403, .F. ) ;
#12258 = CYLINDRICAL_SURFACE ( 'NONE', #5879, 12.00000000000000000 ) ;
#12259 = VERTEX_POINT ( 'NONE', #14997 ) ;
#12260 = EDGE_CURVE ( 'NONE', #20991, #5507, #8336, .T. ) ;
#12261 = ORIENTED_EDGE ( 'NONE', *, *, #7416, .F. ) ;
#12262 = ORIENTED_EDGE ( 'NONE', *, *, #17805, .T. ) ;
#12263 = AXIS2_PLACEMENT_3D ( 'NONE', #9953, #18268, #8198 ) ;
#12264 = CYLINDRICAL_SURFACE ( 'NONE', #19783, 45.00000000000000000 ) ;
#12265 = VERTEX_POINT ( 'NONE', #3185 ) ;
#12266 = AXIS2_PLACEMENT_3D ( 'NONE', #1805, #11969, #3572 ) ;
#12267 = AXIS2_PLACEMENT_3D ( 'NONE', #4372, #11000, #19621 ) ;
#12268 = VERTEX_POINT ( 'NONE', #4425 ) ;
#12269 = AXIS2_PLACEMENT_3D ( 'NONE', #20370, #5228, #11967 ) ;
#12270 = EDGE_CURVE ( 'NONE', #142, #15171, #16751, .T. ) ;
#12271 = CARTESIAN_POINT ( 'NONE',  ( -8.900000000000012790, 1.238117913937974462E-14, 101.1000000000000369 ) ) ;
#12272 = ORIENTED_EDGE ( 'NONE', *, *, #14067, .F. ) ;
#12273 = CARTESIAN_POINT ( 'NONE',  ( 10.00000000000000000, -35.18804927320584142, 80.65854690202667143 ) ) ;
#12274 = CARTESIAN_POINT ( 'NONE',  ( 5.000000000000002665, 85.54350296776139828, -20.64725405482769460 ) ) ;
#12275 = EDGE_CURVE ( 'NONE', #11314, #18794, #16092, .T. ) ;
#12276 = CARTESIAN_POINT ( 'NONE',  ( 10.00000000000000000, -27.00677879429080974, 80.65868421664423238 ) ) ;
#12277 = LINE ( 'NONE', #1798, #14390 ) ;
#12278 = DIRECTION ( 'NONE',  ( -1.000000000000000000, 0.000000000000000000, 0.000000000000000000 ) ) ;
#12279 = CARTESIAN_POINT ( 'NONE',  ( 10.00000000000000000, 87.96697768756401103, -2.410567674970879981 ) ) ;
#12280 = FACE_OUTER_BOUND ( 'NONE', #20183, .T. ) ;
#12281 = DIRECTION ( 'NONE',  ( -1.000000000000000000, 0.000000000000000000, 0.000000000000000000 ) ) ;
#12282 = VECTOR ( 'NONE', #12703, 1000.000000000000000 ) ;
#12283 = AXIS2_PLACEMENT_3D ( 'NONE', #15398, #12084, #13754 ) ;
#12284 = AXIS2_PLACEMENT_3D ( 'NONE', #12390, #1019, #583 ) ;
#12285 = AXIS2_PLACEMENT_3D ( 'NONE', #11181, #15835, #698 ) ;
#12286 = ORIENTED_EDGE ( 'NONE', *, *, #3840, .T. ) ;
#12287 = CIRCLE ( 'NONE', #19706, 32.00000000000000000 ) ;
#12288 = EDGE_CURVE ( 'NONE', #20720, #17060, #20298, .T. ) ;
#12289 = EDGE_CURVE ( 'NONE', #20360, #16931, #19571, .T. ) ;
#12290 = EDGE_CURVE ( 'NONE', #9822, #2850, #2683, .T. ) ;
#12291 = DIRECTION ( 'NONE',  ( -1.000000000000000000, -0.000000000000000000, -0.000000000000000000 ) ) ;
#12292 = ADVANCED_FACE ( 'NONE', ( #14482, #16135 ), #7746, .T. ) ;
#12293 = CARTESIAN_POINT ( 'NONE',  ( 0.000000000000000000, -27.82509854686814066, 4.525913221811051379 ) ) ;
#12294 = EDGE_LOOP ( 'NONE', ( #1905, #7654, #7494, #7255 ) ) ;
#12295 = DIRECTION ( 'NONE',  ( 0.000000000000000000, 0.000000000000000000, 1.000000000000000000 ) ) ;
#12296 = ORIENTED_EDGE ( 'NONE', *, *, #1888, .T. ) ;
#12297 = SURFACE_STYLE_FILL_AREA ( #14162 ) ;
#12298 = CIRCLE ( 'NONE', #5607, 44.99999999999999289 ) ;
#12299 = DIRECTION ( 'NONE',  ( 1.000000000000000000, 0.000000000000000000, 0.000000000000000000 ) ) ;
#12300 = ORIENTED_EDGE ( 'NONE', *, *, #12138, .F. ) ;
#12301 = ORIENTED_EDGE ( 'NONE', *, *, #1771, .T. ) ;
#12302 = CARTESIAN_POINT ( 'NONE',  ( 10.00000000000000000, 88.70892494636771630, -26.21376805916497332 ) ) ;
#12303 = AXIS2_PLACEMENT_3D ( 'NONE', #6395, #13105, #19844 ) ;
#12304 = CARTESIAN_POINT ( 'NONE',  ( 10.00000000000000000, 57.53593069156372053, 72.42963261300981515 ) ) ;
#12305 = CIRCLE ( 'NONE', #11619, 123.0000000000000000 ) ;
#12306 = EDGE_CURVE ( 'NONE', #15663, #18016, #12870, .T. ) ;
#12307 = FACE_OUTER_BOUND ( 'NONE', #10562, .T. ) ;
#12308 = DIRECTION ( 'NONE',  ( -1.000000000000000000, 0.000000000000000000, 0.000000000000000000 ) ) ;
#12309 = DIRECTION ( 'NONE',  ( 0.000000000000000000, 0.000000000000000000, 1.000000000000000000 ) ) ;
#12310 = CARTESIAN_POINT ( 'NONE',  ( 10.00000000000000000, -78.80192417387900150, -39.16958956249377621 ) ) ;
#12311 = DIRECTION ( 'NONE',  ( 1.000000000000000000, 0.000000000000000000, 0.000000000000000000 ) ) ;
#12312 = EDGE_CURVE ( 'NONE', #5510, #1263, #2285, .T. ) ;
#12313 = CYLINDRICAL_SURFACE ( 'NONE', #21129, 88.00000000000000000 ) ;
#12314 = ORIENTED_EDGE ( 'NONE', *, *, #1411, .T. ) ;
#12315 = DIRECTION ( 'NONE',  ( 0.000000000000000000, 0.000000000000000000, -1.000000000000000000 ) ) ;
#12316 = AXIS2_PLACEMENT_3D ( 'NONE', #17764, #19307, #11239 ) ;
#12317 = ORIENTED_EDGE ( 'NONE', *, *, #7167, .F. ) ;
#12318 = VECTOR ( 'NONE', #10556, 1000.000000000000000 ) ;
#12319 = AXIS2_PLACEMENT_3D ( 'NONE', #18010, #8062, #1525 ) ;
#12320 = DIRECTION ( 'NONE',  ( -1.000000000000000000, 0.000000000000000000, 0.000000000000000000 ) ) ;
#12321 = ORIENTED_EDGE ( 'NONE', *, *, #11524, .T. ) ;
#12322 = EDGE_CURVE ( 'NONE', #971, #1655, #16807, .T. ) ;
#12323 = CARTESIAN_POINT ( 'NONE',  ( 150.0000507999999968, 0.000000000000000000, 1.000000000000000000 ) ) ;
#12324 = CARTESIAN_POINT ( 'NONE',  ( 10.00000000000000000, 8.925965667930086056, -92.06933331948771126 ) ) ;
#12325 = ORIENTED_EDGE ( 'NONE', *, *, #17618, .T. ) ;
#12326 = FILL_AREA_STYLE ('',( #8998 ) ) ;
#12327 = ORIENTED_EDGE ( 'NONE', *, *, #7160, .T. ) ;
#12328 = ORIENTED_EDGE ( 'NONE', *, *, #13477, .T. ) ;
#12329 = EDGE_LOOP ( 'NONE', ( #19101, #5103, #7430, #18705 ) ) ;
#12330 = DIRECTION ( 'NONE',  ( 0.000000000000000000, -0.7431448254774000173, 0.6691306063588519093 ) ) ;
#12331 = ORIENTED_EDGE ( 'NONE', *, *, #5432, .F. ) ;
#12332 = CIRCLE ( 'NONE', #2215, 44.99999999999998579 ) ;
#12333 = EDGE_CURVE ( 'NONE', #14447, #21500, #11796, .T. ) ;
#12334 = CYLINDRICAL_SURFACE ( 'NONE', #4021, 92.50100000000000477 ) ;
#12335 = CARTESIAN_POINT ( 'NONE',  ( 10.00000000000000000, -51.18896083639217665, -71.57995730992236361 ) ) ;
#12336 = CARTESIAN_POINT ( 'NONE',  ( 10.00000000000000000, 0.000000000000000000, 0.000000000000000000 ) ) ;
#12337 = VECTOR ( 'NONE', #6899, 1000.000000000000000 ) ;
#12338 = ADVANCED_FACE ( 'NONE', ( #18438 ), #19632, .T. ) ;
#12339 = CIRCLE ( 'NONE', #2816, 7.500000000000021316 ) ;
#12340 = DIRECTION ( 'NONE',  ( -1.000000000000000000, -0.000000000000000000, 0.000000000000000000 ) ) ;
#12341 = DIRECTION ( 'NONE',  ( 0.000000000000000000, 0.000000000000000000, -1.000000000000000000 ) ) ;
#12342 = CARTESIAN_POINT ( 'NONE',  ( 10.00000000000000000, 74.74361964203228581, -40.60271866773572214 ) ) ;
#12343 = ADVANCED_FACE ( 'NONE', ( #16767 ), #8375, .F. ) ;
#12344 = ORIENTED_EDGE ( 'NONE', *, *, #20048, .F. ) ;
#12345 = ADVANCED_FACE ( 'NONE', ( #18543 ), #18655, .F. ) ;
#12346 = CARTESIAN_POINT ( 'NONE',  ( 7.395799999999999486, 0.000000000000000000, -105.0992000000000104 ) ) ;
#12347 = CARTESIAN_POINT ( 'NONE',  ( 1.500000000000001332, 0.000000000000000000, 0.000000000000000000 ) ) ;
#12348 = CARTESIAN_POINT ( 'NONE',  ( 10.00000000000000000, 0.000000000000000000, 0.000000000000000000 ) ) ;
#12349 = VERTEX_POINT ( 'NONE', #3510 ) ;
#12350 = LINE ( 'NONE', #10905, #18336 ) ;
#12351 = ORIENTED_EDGE ( 'NONE', *, *, #15837, .T. ) ;
#12352 = AXIS2_PLACEMENT_3D ( 'NONE', #4885, #16692, #18472 ) ;
#12353 = CARTESIAN_POINT ( 'NONE',  ( 10.00000000000000000, -9.366510754379051562, -25.85466064925435603 ) ) ;
#12354 = ORIENTED_EDGE ( 'NONE', *, *, #9230, .T. ) ;
#12355 = ORIENTED_EDGE ( 'NONE', *, *, #16759, .F. ) ;
#12356 = ORIENTED_EDGE ( 'NONE', *, *, #8004, .T. ) ;
#12357 = LINE ( 'NONE', #19099, #3733 ) ;
#12358 = ORIENTED_EDGE ( 'NONE', *, *, #20511, .T. ) ;
#12359 = CYLINDRICAL_SURFACE ( 'NONE', #18675, 92.50100000000000477 ) ;
#12360 = CARTESIAN_POINT ( 'NONE',  ( 10.00000000000000000, -31.15801000616886896, 79.14775961996379294 ) ) ;
#12361 = CARTESIAN_POINT ( 'NONE',  ( 10.00000000000000000, 61.71252885873388294, 58.53847642588613809 ) ) ;
#12362 = CARTESIAN_POINT ( 'NONE',  ( 10.00000000000000000, 79.38136668499741688, 37.98155635597341728 ) ) ;
#12363 = CARTESIAN_POINT ( 'NONE',  ( 10.00000000000000000, -27.07404830566967746, -4.815694066514710769 ) ) ;
#12364 = FACE_OUTER_BOUND ( 'NONE', #2969, .T. ) ;
#12365 = DIRECTION ( 'NONE',  ( -1.000000000000000000, -0.000000000000000000, -0.000000000000000000 ) ) ;
#12366 = AXIS2_PLACEMENT_3D ( 'NONE', #788, #21456, #19576 ) ;
#12367 = DIRECTION ( 'NONE',  ( -1.000000000000000000, 0.000000000000000000, 0.000000000000000000 ) ) ;
#12368 = CARTESIAN_POINT ( 'NONE',  ( 0.000000000000000000, 0.000000000000000000, 0.000000000000000000 ) ) ;
#12369 = VERTEX_POINT ( 'NONE', #20738 ) ;
#12370 = DIRECTION ( 'NONE',  ( 1.000000000000000000, 0.000000000000000000, 0.000000000000000000 ) ) ;
#12371 = VERTEX_POINT ( 'NONE', #3833 ) ;
#12372 = VERTEX_POINT ( 'NONE', #6947 ) ;
#12373 = VERTEX_POINT ( 'NONE', #5176 ) ;
#12374 = CARTESIAN_POINT ( 'NONE',  ( 0.000000000000000000, 0.000000000000000000, 3.000000000000000000 ) ) ;
#12375 = ORIENTED_EDGE ( 'NONE', *, *, #12182, .T. ) ;
#12376 = ORIENTED_EDGE ( 'NONE', *, *, #10633, .T. ) ;
#12377 = LINE ( 'NONE', #19122, #9815 ) ;
#12378 = EDGE_LOOP ( 'NONE', ( #240, #15713, #6799, #4562 ) ) ;
#12379 = DIRECTION ( 'NONE',  ( -1.000000000000000000, -0.000000000000000000, -0.000000000000000000 ) ) ;
#12380 = CYLINDRICAL_SURFACE ( 'NONE', #17022, 27.49900000000000233 ) ;
#12381 = CYLINDRICAL_SURFACE ( 'NONE', #13584, 44.99999999999998579 ) ;
#12382 = CARTESIAN_POINT ( 'NONE',  ( 10.00000000000000000, 84.12297548659721258, -12.59025161327029529 ) ) ;
#12383 = ADVANCED_FACE ( 'NONE', ( #3722 ), #17319, .F. ) ;
#12384 = CARTESIAN_POINT ( 'NONE',  ( 10.00000000000000000, -40.72878876293203376, 78.00747250042435610 ) ) ;
#12385 = DIRECTION ( 'NONE',  ( -1.000000000000000000, 0.000000000000000000, 0.000000000000000000 ) ) ;
#12386 = DIRECTION ( 'NONE',  ( 0.000000000000000000, 0.000000000000000000, 1.000000000000000000 ) ) ;
#12387 = FACE_OUTER_BOUND ( 'NONE', #16263, .T. ) ;
#12388 = ORIENTED_EDGE ( 'NONE', *, *, #8406, .T. ) ;
#12389 = EDGE_CURVE ( 'NONE', #17888, #11293, #19230, .T. ) ;
#12390 = CARTESIAN_POINT ( 'NONE',  ( 10.00000000000000000, -84.90234713953988432, 5.175025661883520200 ) ) ;
#12391 = CARTESIAN_POINT ( 'NONE',  ( 0.000000000000000000, 18.31866948046803145, -26.23788002993705248 ) ) ;
#12392 = ORIENTED_EDGE ( 'NONE', *, *, #10900, .T. ) ;
#12393 = CARTESIAN_POINT ( 'NONE',  ( 10.00000000000000000, -64.66851233300690183, -55.25552418573029456 ) ) ;
#12394 = EDGE_LOOP ( 'NONE', ( #9846, #4994, #9241, #7278 ) ) ;
#12395 =( NAMED_UNIT ( * ) PLANE_ANGLE_UNIT ( ) SI_UNIT ( $, .RADIAN. ) );
#12396 = LINE ( 'NONE', #20589, #7174 ) ;
#12397 = ORIENTED_EDGE ( 'NONE', *, *, #20816, .T. ) ;
#12398 = CIRCLE ( 'NONE', #15225, 5.000000000000000000 ) ;
#12399 = ORIENTED_EDGE ( 'NONE', *, *, #13221, .F. ) ;
#12400 = CARTESIAN_POINT ( 'NONE',  ( 5.000000000000002665, 5.479102470010468018, 87.82926298292115064 ) ) ;
#12401 = DIRECTION ( 'NONE',  ( -1.000000000000000000, -0.000000000000000000, -0.000000000000000000 ) ) ;
#12402 = LINE ( 'NONE', #19151, #14746 ) ;
#12403 = EDGE_CURVE ( 'NONE', #8003, #1184, #11472, .T. ) ;
#12404 = EDGE_CURVE ( 'NONE', #10332, #12482, #20996, .T. ) ;
#12405 = CARTESIAN_POINT ( 'NONE',  ( 0.000000000000000000, -23.37352460145298139, 21.85585385440871775 ) ) ;
#12406 = CARTESIAN_POINT ( 'NONE',  ( 0.000000000000000000, 0.000000000000000000, -3.000000000000000000 ) ) ;
#12407 = CARTESIAN_POINT ( 'NONE',  ( 10.00000000000000000, -16.79755869217588682, -90.96305306542271296 ) ) ;
#12408 = DIRECTION ( 'NONE',  ( 1.000000000000000000, 0.000000000000000000, 0.000000000000000000 ) ) ;
#12409 = EDGE_CURVE ( 'NONE', #5185, #9562, #13231, .T. ) ;
#12410 = ORIENTED_EDGE ( 'NONE', *, *, #20124, .T. ) ;
#12411 = LINE ( 'NONE', #496, #5812 ) ;
#12412 = ORIENTED_EDGE ( 'NONE', *, *, #3920, .F. ) ;
#12413 = DIRECTION ( 'NONE',  ( 0.000000000000000000, 0.000000000000000000, -1.000000000000000000 ) ) ;
#12414 = ADVANCED_FACE ( 'NONE', ( #5283 ), #16053, .T. ) ;
#12415 = ORIENTED_EDGE ( 'NONE', *, *, #20048, .T. ) ;
#12416 = CARTESIAN_POINT ( 'NONE',  ( 10.00000000000000000, 0.000000000000000000, 0.000000000000000000 ) ) ;
#12417 = CIRCLE ( 'NONE', #17372, 27.49900000000000233 ) ;
#12418 = DIRECTION ( 'NONE',  ( 1.000000000000000000, -0.000000000000000000, -0.000000000000000000 ) ) ;
#12419 = ORIENTED_EDGE ( 'NONE', *, *, #8934, .T. ) ;
#12420 = PRESENTATION_STYLE_ASSIGNMENT (( #10559 ) ) ;
#12421 = ADVANCED_FACE ( 'NONE', ( #13781 ), #2071, .F. ) ;
#12422 = VERTEX_POINT ( 'NONE', #2273 ) ;
#12423 = VECTOR ( 'NONE', #2243, 1000.000000000000000 ) ;
#12424 = VERTEX_POINT ( 'NONE', #12113 ) ;
#12425 = VERTEX_POINT ( 'NONE', #7263 ) ;
#12426 = CARTESIAN_POINT ( 'NONE',  ( 5.000000000000002665, -87.44637528609653998, -9.855528870799531660 ) ) ;
#12427 = CARTESIAN_POINT ( 'NONE',  ( 0.000000000000000000, 0.000000000000000000, 15.00000000000000000 ) ) ;
#12428 = AXIS2_PLACEMENT_3D ( 'NONE', #4730, #3188, #11471 ) ;
#12429 = VERTEX_POINT ( 'NONE', #13877 ) ;
#12430 = DIRECTION ( 'NONE',  ( 0.000000000000000000, 0.000000000000000000, 1.000000000000000000 ) ) ;
#12431 = DIRECTION ( 'NONE',  ( -1.000000000000000000, -0.000000000000000000, 0.000000000000000000 ) ) ;
#12432 = CARTESIAN_POINT ( 'NONE',  ( 10.00000000000000000, 0.000000000000000000, 0.000000000000000000 ) ) ;
#12433 = ADVANCED_FACE ( 'NONE', ( #5381 ), #20623, .T. ) ;
#12434 = CARTESIAN_POINT ( 'NONE',  ( 10.00000000000000000, -9.646732466565913100, 84.51112348751846071 ) ) ;
#12435 = CARTESIAN_POINT ( 'NONE',  ( 0.000000000000000000, 0.000000000000000000, 0.000000000000000000 ) ) ;
#12436 = ADVANCED_FACE ( 'NONE', ( #19081 ), #18754, .F. ) ;
#12437 = AXIS2_PLACEMENT_3D ( 'NONE', #8508, #9935, #8292 ) ;
#12438 = ORIENTED_EDGE ( 'NONE', *, *, #1886, .T. ) ;
#12439 = DIRECTION ( 'NONE',  ( -0.000000000000000000, -1.000000000000000000, -0.000000000000000000 ) ) ;
#12440 = CARTESIAN_POINT ( 'NONE',  ( 0.000000000000000000, 0.000000000000000000, 0.000000000000000000 ) ) ;
#12441 = AXIS2_PLACEMENT_3D ( 'NONE', #21699, #21590, #3578 ) ;
#12442 = DIRECTION ( 'NONE',  ( -1.000000000000000000, -0.000000000000000000, -0.000000000000000000 ) ) ;
#12443 = EDGE_CURVE ( 'NONE', #12017, #17170, #20651, .T. ) ;
#12444 = ORIENTED_EDGE ( 'NONE', *, *, #15946, .F. ) ;
#12445 = CARTESIAN_POINT ( 'NONE',  ( 8.899999999999989697, 0.000000000000000000, 0.000000000000000000 ) ) ;
#12446 = ORIENTED_EDGE ( 'NONE', *, *, #3920, .T. ) ;
#12447 = LINE ( 'NONE', #19095, #4184 ) ;
#12448 = EDGE_CURVE ( 'NONE', #10147, #8155, #6198, .T. ) ;
#12449 = ORIENTED_EDGE ( 'NONE', *, *, #4346, .T. ) ;
#12450 = CIRCLE ( 'NONE', #19522, 88.00000000000000000 ) ;
#12451 = ORIENTED_EDGE ( 'NONE', *, *, #5464, .F. ) ;
#12452 = EDGE_LOOP ( 'NONE', ( #3763, #1894, #16930, #11593 ) ) ;
#12453 = CARTESIAN_POINT ( 'NONE',  ( 10.00000000000000000, -84.33453774737664332, 11.08490790852103380 ) ) ;
#12454 = EDGE_CURVE ( 'NONE', #11232, #18476, #8305, .T. ) ;
#12455 = VERTEX_POINT ( 'NONE', #13991 ) ;
#12456 = CARTESIAN_POINT ( 'NONE',  ( 10.00000000000000000, -47.19205848891816402, 74.27590198428104884 ) ) ;
#12457 = VECTOR ( 'NONE', #2521, 1000.000000000000000 ) ;
#12458 = AXIS2_PLACEMENT_3D ( 'NONE', #13014, #1084, #14669 ) ;
#12459 = DIRECTION ( 'NONE',  ( -1.000000000000000000, -0.000000000000000000, 0.000000000000000000 ) ) ;
#12460 = LINE ( 'NONE', #8832, #7152 ) ;
#12461 = DIRECTION ( 'NONE',  ( -1.000000000000000000, -0.000000000000000000, -0.000000000000000000 ) ) ;
#12462 = CIRCLE ( 'NONE', #19880, 44.99999999999999289 ) ;
#12463 = CONICAL_SURFACE ( 'NONE', #13886, 5.612499999999999822, 0.4883339510564123076 ) ;
#12464 = DIRECTION ( 'NONE',  ( -1.000000000000000000, 0.000000000000000000, -0.000000000000000000 ) ) ;
#12465 = EDGE_CURVE ( 'NONE', #15522, #9323, #9688, .T. ) ;
#12466 = CARTESIAN_POINT ( 'NONE',  ( 10.00000000000000000, 37.96946988134275358, -76.11510229470822253 ) ) ;
#12467 = DIRECTION ( 'NONE',  ( 0.000000000000000000, 0.000000000000000000, 1.000000000000000000 ) ) ;
#12468 = CARTESIAN_POINT ( 'NONE',  ( 10.00000000000000000, 0.000000000000000000, 0.000000000000000000 ) ) ;
#12469 = FACE_OUTER_BOUND ( 'NONE', #19120, .T. ) ;
#12470 = CIRCLE ( 'NONE', #20602, 44.99999999999999289 ) ;
#12471 = ORIENTED_EDGE ( 'NONE', *, *, #18242, .F. ) ;
#12472 = CYLINDRICAL_SURFACE ( 'NONE', #11520, 88.00000000000000000 ) ;
#12473 = AXIS2_PLACEMENT_3D ( 'NONE', #250, #15374, #6996 ) ;
#12474 = ORIENTED_EDGE ( 'NONE', *, *, #11721, .T. ) ;
#12475 = ORIENTED_EDGE ( 'NONE', *, *, #9867, .F. ) ;
#12476 = VERTEX_POINT ( 'NONE', #625 ) ;
#12477 = VERTEX_POINT ( 'NONE', #20950 ) ;
#12478 = ORIENTED_EDGE ( 'NONE', *, *, #11716, .T. ) ;
#12479 = EDGE_CURVE ( 'NONE', #18348, #4328, #17492, .T. ) ;
#12480 = ORIENTED_EDGE ( 'NONE', *, *, #4715, .T. ) ;
#12481 = CARTESIAN_POINT ( 'NONE',  ( 0.000000000000000000, 16.79755869217770936, -90.96305306542237190 ) ) ;
#12482 = VERTEX_POINT ( 'NONE', #9548 ) ;
#12483 = DIRECTION ( 'NONE',  ( 0.000000000000000000, -0.06975647374413235235, 0.9975640502598237536 ) ) ;
#12484 = DIRECTION ( 'NONE',  ( 0.000000000000000000, 0.000000000000000000, 1.000000000000000000 ) ) ;
#12485 = CARTESIAN_POINT ( 'NONE',  ( 0.000000000000000000, 17.83210509884670714, -21.83428559348744002 ) ) ;
#12486 = LINE ( 'NONE', #14486, #13504 ) ;
#12487 = FACE_OUTER_BOUND ( 'NONE', #17661, .T. ) ;
#12488 = AXIS2_PLACEMENT_3D ( 'NONE', #19372, #10532, #10423 ) ;
#12489 = CARTESIAN_POINT ( 'NONE',  ( 10.00000000000000000, 0.000000000000000000, 0.000000000000000000 ) ) ;
#12490 = DIRECTION ( 'NONE',  ( -1.000000000000000000, -0.000000000000000000, -0.000000000000000000 ) ) ;
#12491 = DIRECTION ( 'NONE',  ( 0.000000000000000000, -0.9945218953682722907, -0.1045284632676635739 ) ) ;
#12492 = VERTEX_POINT ( 'NONE', #7581 ) ;
#12493 = DIRECTION ( 'NONE',  ( 1.000000000000000000, 0.000000000000000000, 0.000000000000000000 ) ) ;
#12494 = AXIS2_PLACEMENT_3D ( 'NONE', #5088, #18577, #16915 ) ;
#12495 = CIRCLE ( 'NONE', #3034, 44.99999999999999289 ) ;
#12496 = FACE_OUTER_BOUND ( 'NONE', #498, .T. ) ;
#12497 = CIRCLE ( 'NONE', #17460, 88.00000000000000000 ) ;
#12498 = CARTESIAN_POINT ( 'NONE',  ( 5.000000000000000888, -0.6021240089799216877, -31.99433460282945063 ) ) ;
#12499 = ORIENTED_EDGE ( 'NONE', *, *, #8531, .T. ) ;
#12500 = DIRECTION ( 'NONE',  ( 0.000000000000000000, 0.000000000000000000, -1.000000000000000000 ) ) ;
#12501 = EDGE_LOOP ( 'NONE', ( #10238, #17477, #14116, #12125 ) ) ;
#12502 = AXIS2_PLACEMENT_3D ( 'NONE', #7079, #13805, #20546 ) ;
#12503 = FILL_AREA_STYLE_COLOUR ( '', #1116 ) ;
#12504 = DIRECTION ( 'NONE',  ( 0.000000000000000000, 0.000000000000000000, 1.000000000000000000 ) ) ;
#12505 = ORIENTED_EDGE ( 'NONE', *, *, #2940, .F. ) ;
#12506 = ORIENTED_EDGE ( 'NONE', *, *, #5982, .T. ) ;
#12507 = DIRECTION ( 'NONE',  ( 1.000000000000000000, 0.000000000000000000, 0.000000000000000000 ) ) ;
#12508 = PRODUCT_DEFINITION ( 'UNKNOWN', '', #1133, #7175 ) ;
#12509 = CARTESIAN_POINT ( 'NONE',  ( 10.00000000000000000, 0.6609040254623582689, -87.99751818016873983 ) ) ;
#12510 = CIRCLE ( 'NONE', #15338, 114.9007999999999896 ) ;
#12511 = CARTESIAN_POINT ( 'NONE',  ( 10.00000000000000000, -51.10509369859380513, -77.10190917907254970 ) ) ;
#12512 = DIRECTION ( 'NONE',  ( 0.000000000000000000, 0.000000000000000000, 1.000000000000000000 ) ) ;
#12513 = CIRCLE ( 'NONE', #523, 88.00000000000000000 ) ;
#12514 = DIRECTION ( 'NONE',  ( 0.000000000000000000, 0.000000000000000000, 1.000000000000000000 ) ) ;
#12515 = FACE_OUTER_BOUND ( 'NONE', #21521, .T. ) ;
#12516 = AXIS2_PLACEMENT_3D ( 'NONE', #7053, #10669, #514 ) ;
#12517 = DIRECTION ( 'NONE',  ( -0.000000000000000000, -0.000000000000000000, 1.000000000000000000 ) ) ;
#12518 = DIRECTION ( 'NONE',  ( -1.000000000000000000, 0.000000000000000000, -0.000000000000000000 ) ) ;
#12520 = AXIS2_PLACEMENT_3D ( 'NONE', #1360, #17827, #16602 ) ;
#12519 = DIRECTION ( 'NONE',  ( 0.000000000000000000, 0.5877852522924689183, 0.8090169943749504489 ) ) ;
#12521 = ORIENTED_EDGE ( 'NONE', *, *, #2281, .T. ) ;
#12522 = AXIS2_PLACEMENT_3D ( 'NONE', #17235, #2097, #8831 ) ;
#12523 = CYLINDRICAL_SURFACE ( 'NONE', #15372, 92.50100000000000477 ) ;
#12524 = VERTEX_POINT ( 'NONE', #14316 ) ;
#12525 = VECTOR ( 'NONE', #1596, 1000.000000000000000 ) ;
#12526 = CYLINDRICAL_SURFACE ( 'NONE', #21093, 44.99999999999999289 ) ;
#12527 = VERTEX_POINT ( 'NONE', #2601 ) ;
#12528 = DIRECTION ( 'NONE',  ( 0.000000000000000000, 0.000000000000000000, 1.000000000000000000 ) ) ;
#12529 = EDGE_CURVE ( 'NONE', #3876, #21664, #19247, .T. ) ;
#12530 = AXIS2_PLACEMENT_3D ( 'NONE', #8000, #8441, #21581 ) ;
#12531 = AXIS2_PLACEMENT_3D ( 'NONE', #21608, #15083, #14651 ) ;
#12532 = DIRECTION ( 'NONE',  ( 1.000000000000000000, 0.000000000000000000, 0.000000000000000000 ) ) ;
#12533 = ORIENTED_EDGE ( 'NONE', *, *, #12818, .F. ) ;
#12534 = VECTOR ( 'NONE', #19478, 1000.000000000000000 ) ;
#12535 = SURFACE_SIDE_STYLE ('',( #4029 ) ) ;
#12536 = AXIS2_PLACEMENT_3D ( 'NONE', #4755, #12808, #2654 ) ;
#12537 = ORIENTED_EDGE ( 'NONE', *, *, #5847, .F. ) ;
#12538 = VERTEX_POINT ( 'NONE', #14203 ) ;
#12539 = EDGE_LOOP ( 'NONE', ( #7305, #1995, #7896, #996 ) ) ;
#12540 = CARTESIAN_POINT ( 'NONE',  ( 0.000000000000000000, 15.00000000000000000, 0.000000000000000000 ) ) ;
#12541 = CARTESIAN_POINT ( 'NONE',  ( 10.00000000000000000, -88.70892494636754577, 26.21376805916555242 ) ) ;
#12542 = ADVANCED_FACE ( 'NONE', ( #6046 ), #1062, .F. ) ;
#12543 = ORIENTED_EDGE ( 'NONE', *, *, #2878, .F. ) ;
#12544 = DIRECTION ( 'NONE',  ( -1.000000000000000000, -0.000000000000000000, -0.000000000000000000 ) ) ;
#12545 = PLANE ( 'NONE',  #11569 ) ;
#12546 = DIRECTION ( 'NONE',  ( 0.000000000000000000, 0.000000000000000000, -1.000000000000000000 ) ) ;
#12547 = DIRECTION ( 'NONE',  ( 1.000000000000000000, 0.000000000000000000, 0.000000000000000000 ) ) ;
#12548 = CARTESIAN_POINT ( 'NONE',  ( -5.000000000000000000, 67.00000000000000000, 9.999999999999998224 ) ) ;
#12549 = ADVANCED_FACE ( 'NONE', ( #5929 ), #736, .T. ) ;
#12550 = AXIS2_PLACEMENT_3D ( 'NONE', #14493, #6101, #2992 ) ;
#12551 = ORIENTED_EDGE ( 'NONE', *, *, #18013, .T. ) ;
#12552 = AXIS2_PLACEMENT_3D ( 'NONE', #19946, #18306, #16634 ) ;
#12553 = CARTESIAN_POINT ( 'NONE',  ( -10.00000000000000000, 0.000000000000000000, 0.000000000000000000 ) ) ;
#12554 = CIRCLE ( 'NONE', #21382, 92.50100000000000477 ) ;
#12555 = DIRECTION ( 'NONE',  ( -1.000000000000000000, -0.000000000000000000, -0.000000000000000000 ) ) ;
#12556 = ORIENTED_EDGE ( 'NONE', *, *, #19060, .T. ) ;
#12557 = EDGE_CURVE ( 'NONE', #12259, #966, #2829, .T. ) ;
#12558 = DIRECTION ( 'NONE',  ( 0.000000000000000000, 0.000000000000000000, 1.000000000000000000 ) ) ;
#12559 = EDGE_CURVE ( 'NONE', #7099, #4539, #7592, .T. ) ;
#12560 = EDGE_CURVE ( 'NONE', #20636, #1054, #5832, .T. ) ;
#12561 = ORIENTED_EDGE ( 'NONE', *, *, #2736, .F. ) ;
#12562 = DIRECTION ( 'NONE',  ( 0.000000000000000000, 0.7880107536067231244, -0.6156614753256566264 ) ) ;
#12563 = EDGE_LOOP ( 'NONE', ( #7413, #3737, #3871, #3196 ) ) ;
#12564 = EDGE_CURVE ( 'NONE', #6526, #5435, #19943, .T. ) ;
#12565 = VERTEX_POINT ( 'NONE', #10891 ) ;
#12566 = CIRCLE ( 'NONE', #1994, 88.00000000000000000 ) ;
#12567 = ORIENTED_EDGE ( 'NONE', *, *, #3505, .F. ) ;
#12568 = LINE ( 'NONE', #4067, #13265 ) ;
#12569 = AXIS2_PLACEMENT_3D ( 'NONE', #3126, #19919, #21473 ) ;
#12570 = ORIENTED_EDGE ( 'NONE', *, *, #19051, .T. ) ;
#12571 = VECTOR ( 'NONE', #10671, 1000.000000000000000 ) ;
#12572 = DIRECTION ( 'NONE',  ( 1.000000000000000000, 0.000000000000000000, 0.000000000000000000 ) ) ;
#12573 = CARTESIAN_POINT ( 'NONE',  ( 0.000000000000000000, -25.48117629651182270, -10.33947075754286793 ) ) ;
#12574 = CYLINDRICAL_SURFACE ( 'NONE', #2228, 11.99999999999999645 ) ;
#12575 = CARTESIAN_POINT ( 'NONE',  ( 0.000000000000000000, -52.25832601289145884, 70.80301803122767978 ) ) ;
#12576 = ADVANCED_FACE ( 'NONE', ( #11001, #2498 ), #16082, .T. ) ;
#12577 = DIRECTION ( 'NONE',  ( 0.000000000000000000, -0.1391731009600725433, 0.9902680687415692518 ) ) ;
#12578 = CARTESIAN_POINT ( 'NONE',  ( -1.139999999999998570, 0.000000000000000000, 0.000000000000000000 ) ) ;
#12579 = CARTESIAN_POINT ( 'NONE',  ( 10.00000000000000000, 0.000000000000000000, 0.000000000000000000 ) ) ;
#12580 = EDGE_CURVE ( 'NONE', #5874, #9950, #12885, .T. ) ;
#12581 = DIRECTION ( 'NONE',  ( 0.000000000000000000, 0.000000000000000000, 1.000000000000000000 ) ) ;
#12582 = VECTOR ( 'NONE', #213, 1000.000000000000000 ) ;
#12583 = VECTOR ( 'NONE', #9172, 1000.000000000000000 ) ;
#12584 = EDGE_CURVE ( 'NONE', #18503, #12821, #11125, .T. ) ;
#12585 = CYLINDRICAL_SURFACE ( 'NONE', #16802, 12.00000000000000000 ) ;
#12586 = ORIENTED_EDGE ( 'NONE', *, *, #10199, .T. ) ;
#12587 = EDGE_LOOP ( 'NONE', ( #1478, #18564, #15099, #8690 ) ) ;
#12588 = VERTEX_POINT ( 'NONE', #16296 ) ;
#12589 = ADVANCED_FACE ( 'NONE', ( #949 ), #12874, .F. ) ;
#12590 = VERTEX_POINT ( 'NONE', #5708 ) ;
#12591 = ORIENTED_EDGE ( 'NONE', *, *, #10989, .T. ) ;
#12592 = DIRECTION ( 'NONE',  ( 0.000000000000000000, 0.9945218953682729568, 0.1045284632676569958 ) ) ;
#12593 = ORIENTED_EDGE ( 'NONE', *, *, #13462, .T. ) ;
#12594 = CIRCLE ( 'NONE', #11555, 88.00000000000000000 ) ;
#12595 = CARTESIAN_POINT ( 'NONE',  ( 5.000000000000002665, -87.92084725184950855, 3.731570516142653116 ) ) ;
#12596 = DIRECTION ( 'NONE',  ( 0.000000000000000000, 0.000000000000000000, -1.000000000000000000 ) ) ;
#12597 = FACE_OUTER_BOUND ( 'NONE', #3793, .T. ) ;
#12598 = CARTESIAN_POINT ( 'NONE',  ( 0.000000000000000000, 9.366510754379572035, -25.85466064925416774 ) ) ;
#12599 = CARTESIAN_POINT ( 'NONE',  ( 10.00000000000000000, 27.87320266523671819, -88.20158487341731757 ) ) ;
#12600 = EDGE_CURVE ( 'NONE', #7213, #16952, #14428, .T. ) ;
#12601 = DIRECTION ( 'NONE',  ( -1.000000000000000000, 0.000000000000000000, -0.000000000000000000 ) ) ;
#12602 = CARTESIAN_POINT ( 'NONE',  ( 10.00000000000000000, 85.05652083079336023, -0.7600687895862878740 ) ) ;
#12603 = CARTESIAN_POINT ( 'NONE',  ( 0.000000000000000000, 0.000000000000000000, 3.000000000000000000 ) ) ;
#12604 = EDGE_CURVE ( 'NONE', #791, #6638, #3365, .T. ) ;
#12605 = VERTEX_POINT ( 'NONE', #21277 ) ;
#12606 = EDGE_CURVE ( 'NONE', #17077, #8172, #17535, .T. ) ;
#12607 = DIRECTION ( 'NONE',  ( -1.000000000000000000, 0.000000000000000000, 0.000000000000000000 ) ) ;
#12608 = VECTOR ( 'NONE', #553, 1000.000000000000000 ) ;
#12609 = CIRCLE ( 'NONE', #617, 44.99999999999999289 ) ;
#12610 = AXIS2_PLACEMENT_3D ( 'NONE', #6301, #11469, #979 ) ;
#12611 = CARTESIAN_POINT ( 'NONE',  ( 0.000000000000000000, 0.000000000000000000, 0.000000000000000000 ) ) ;
#12612 = DIRECTION ( 'NONE',  ( -1.000000000000000000, 0.000000000000000000, 0.000000000000000000 ) ) ;
#12613 = VECTOR ( 'NONE', #17803, 1000.000000000000000 ) ;
#12614 = ORIENTED_EDGE ( 'NONE', *, *, #17184, .F. ) ;
#12615 = DIRECTION ( 'NONE',  ( 0.000000000000000000, 0.000000000000000000, 1.000000000000000000 ) ) ;
#12616 = ORIENTED_EDGE ( 'NONE', *, *, #12033, .F. ) ;
#12617 = CARTESIAN_POINT ( 'NONE',  ( 0.000000000000000000, -90.63195040374175449, -18.50093422002511900 ) ) ;
#12618 = ORIENTED_EDGE ( 'NONE', *, *, #8964, .F. ) ;
#12619 = ORIENTED_EDGE ( 'NONE', *, *, #14325, .T. ) ;
#12620 = DIRECTION ( 'NONE',  ( -1.000000000000000000, -0.000000000000000000, -0.000000000000000000 ) ) ;
#12621 = CARTESIAN_POINT ( 'NONE',  ( 0.000000000000000000, -9.366510754379051562, -25.85466064925435603 ) ) ;
#12622 = AXIS2_PLACEMENT_3D ( 'NONE', #7685, #15872, #2380 ) ;
#12623 = VECTOR ( 'NONE', #599, 1000.000000000000000 ) ;
#12624 = DIRECTION ( 'NONE',  ( -0.000000000000000000, -0.000000000000000000, -1.000000000000000000 ) ) ;
#12625 = CARTESIAN_POINT ( 'NONE',  ( 10.00000000000000000, -46.89573839703331259, 79.73220629831473616 ) ) ;
#12626 = AXIS2_PLACEMENT_3D ( 'NONE', #10083, #12069, #16832 ) ;
#12627 = CYLINDRICAL_SURFACE ( 'NONE', #9720, 44.99999999999999289 ) ;
#12628 = CIRCLE ( 'NONE', #19681, 45.00000000000000000 ) ;
#12629 = DIRECTION ( 'NONE',  ( -1.000000000000000000, 0.000000000000000000, 0.000000000000000000 ) ) ;
#12630 = AXIS2_PLACEMENT_3D ( 'NONE', #16387, #1577, #11531 ) ;
#12631 = DIRECTION ( 'NONE',  ( 0.000000000000000000, 0.000000000000000000, 1.000000000000000000 ) ) ;
#12632 = CARTESIAN_POINT ( 'NONE',  ( 0.000000000000000000, -30.61448696004458370, 9.314139153634124924 ) ) ;
#12633 = DIRECTION ( 'NONE',  ( -1.000000000000000000, 0.000000000000000000, 0.000000000000000000 ) ) ;
#12634 = VERTEX_POINT ( 'NONE', #14759 ) ;
#12635 = CARTESIAN_POINT ( 'NONE',  ( 10.00000000000000000, 92.22057093985038989, -7.197311757039552838 ) ) ;
#12636 = ORIENTED_EDGE ( 'NONE', *, *, #16050, .F. ) ;
#12637 = CARTESIAN_POINT ( 'NONE',  ( 10.00000000000000000, -74.39348546125087580, 54.97312363261389834 ) ) ;
#12638 = ORIENTED_EDGE ( 'NONE', *, *, #811, .F. ) ;
#12639 = AXIS2_PLACEMENT_3D ( 'NONE', #4748, #1438, #11492 ) ;
#12640 = SURFACE_SIDE_STYLE ('',( #14742 ) ) ;
#12641 = VECTOR ( 'NONE', #16351, 1000.000000000000000 ) ;
#12642 = AXIS2_PLACEMENT_3D ( 'NONE', #13158, #6340, #19907 ) ;
#12643 = DIRECTION ( 'NONE',  ( -1.000000000000000000, -0.000000000000000000, -0.000000000000000000 ) ) ;
#12644 = CIRCLE ( 'NONE', #17598, 32.00000000000000000 ) ;
#12645 = ORIENTED_EDGE ( 'NONE', *, *, #12021, .T. ) ;
#12646 = ORIENTED_EDGE ( 'NONE', *, *, #16613, .T. ) ;
#12647 = EDGE_LOOP ( 'NONE', ( #6532, #11990, #11237, #20966, #16517, #5096, #12296, #19440, #3547, #8131, #14405, #17966, #8071, #8825, #2925, #14195, #5529, #21829, #10265, #16343, #18883, #17229, #8763, #13073, #9983, #16390, #9459, #1702, #9137, #13859, #12591, #13100, #5040, #19881, #15768, #9976, #8515, #15471, #6339, #9647, #18724, #13624, #4677, #2491, #14081, #4226, #1814, #17818, #8684, #5019, #12410, #12031, #14658, #3771, #5700, #17763, #9005, #9762, #10558, #934, #9024, #11717, #4665, #4149, #11865, #20459, #28, #8582, #9056, #15698, #3193, #9464, #18877, #14871, #19628, #10356, #16653, #9908, #9375, #6050, #17680, #14041, #17225, #2064, #10234, #2213, #1859, #17443, #12325, #19435, #6669, #17612, #818, #18703, #14207, #16124, #17765, #14827, #3303, #1131, #6115, #1839, #8947, #2409, #15892, #14378, #7137, #17525, #4282, #4393, #10518, #19795, #4179, #703, #18376, #6936, #4986, #13242, #7734, #4565, #9694, #689, #12000, #15647, #19333 ) ) ;
#12648 = ORIENTED_EDGE ( 'NONE', *, *, #11328, .T. ) ;
#12649 = CYLINDRICAL_SURFACE ( 'NONE', #19898, 44.99999999999999289 ) ;
#12650 = CARTESIAN_POINT ( 'NONE',  ( 0.000000000000000000, 0.000000000000000000, 0.000000000000000000 ) ) ;
#12651 = ORIENTED_EDGE ( 'NONE', *, *, #2050, .F. ) ;
#12652 = CARTESIAN_POINT ( 'NONE',  ( 10.00000000000000000, -22.77465461094683974, 15.41136296218079238 ) ) ;
#12653 = DIRECTION ( 'NONE',  ( 1.000000000000000000, 0.000000000000000000, 0.000000000000000000 ) ) ;
#12654 = DIRECTION ( 'NONE',  ( -1.000000000000000000, -0.000000000000000000, -0.000000000000000000 ) ) ;
#12655 = AXIS2_PLACEMENT_3D ( 'NONE', #19407, #20953, #11116 ) ;
#12656 = DIRECTION ( 'NONE',  ( 1.000000000000000000, -0.000000000000000000, -0.000000000000000000 ) ) ;
#12657 = DIRECTION ( 'NONE',  ( 1.000000000000000000, 0.000000000000000000, 0.000000000000000000 ) ) ;
#12658 = EDGE_CURVE ( 'NONE', #4022, #1128, #17832, .T. ) ;
#12659 = AXIS2_PLACEMENT_3D ( 'NONE', #11889, #3274, #13437 ) ;
#12660 = CIRCLE ( 'NONE', #11253, 0.02570000000000176310 ) ;
#12661 = ORIENTED_EDGE ( 'NONE', *, *, #7481, .F. ) ;
#12662 = CIRCLE ( 'NONE', #11254, 5.000000000000000000 ) ;
#12663 = CARTESIAN_POINT ( 'NONE',  ( 0.000000000000000000, -88.70892494636720471, -26.21376805916674613 ) ) ;
#12664 = DIRECTION ( 'NONE',  ( 0.000000000000000000, 0.000000000000000000, 1.000000000000000000 ) ) ;
#12665 = EDGE_CURVE ( 'NONE', #13330, #15096, #7252, .T. ) ;
#12666 = FACE_OUTER_BOUND ( 'NONE', #4750, .T. ) ;
#12667 = AXIS2_PLACEMENT_3D ( 'NONE', #15494, #578, #20687 ) ;
#12668 = VERTEX_POINT ( 'NONE', #2929 ) ;
#12669 = CARTESIAN_POINT ( 'NONE',  ( 10.00000000000000000, -7.619321854369744074, 26.42235673590688094 ) ) ;
#12670 = ORIENTED_EDGE ( 'NONE', *, *, #13503, .F. ) ;
#12671 = CARTESIAN_POINT ( 'NONE',  ( 0.000000000000000000, -27.26034713664092379, -7.182859710736426706 ) ) ;
#12672 = ORIENTED_EDGE ( 'NONE', *, *, #3282, .T. ) ;
#12673 = ORIENTED_EDGE ( 'NONE', *, *, #5730, .T. ) ;
#12674 = AXIS2_PLACEMENT_3D ( 'NONE', #820, #15865, #14299 ) ;
#12675 = ORIENTED_EDGE ( 'NONE', *, *, #6217, .T. ) ;
#12676 = VECTOR ( 'NONE', #8993, 1000.000000000000000 ) ;
#12677 = DIRECTION ( 'NONE',  ( -1.000000000000000000, -0.000000000000000000, -0.000000000000000000 ) ) ;
#12678 = AXIS2_PLACEMENT_3D ( 'NONE', #19869, #16564, #1430 ) ;
#12679 = VERTEX_POINT ( 'NONE', #8024 ) ;
#12680 = LINE ( 'NONE', #19421, #4547 ) ;
#12681 = FACE_OUTER_BOUND ( 'NONE', #9515, .T. ) ;
#12682 = DIRECTION ( 'NONE',  ( 0.000000000000000000, 0.000000000000000000, 1.000000000000000000 ) ) ;
#12683 = DIRECTION ( 'NONE',  ( -1.000000000000000000, 0.000000000000000000, 0.000000000000000000 ) ) ;
#12684 = CARTESIAN_POINT ( 'NONE',  ( 10.00000000000000000, 0.000000000000000000, 0.000000000000000000 ) ) ;
#12685 = EDGE_CURVE ( 'NONE', #15558, #15756, #10059, .T. ) ;
#12686 = CARTESIAN_POINT ( 'NONE',  ( 10.00000000000000000, 0.000000000000000000, 0.000000000000000000 ) ) ;
#12687 = EDGE_CURVE ( 'NONE', #18019, #19336, #7955, .T. ) ;
#12688 = DIRECTION ( 'NONE',  ( 0.000000000000000000, 0.000000000000000000, 1.000000000000000000 ) ) ;
#12689 = ADVANCED_FACE ( 'NONE', ( #9887 ), #20169, .F. ) ;
#12690 = DIRECTION ( 'NONE',  ( -1.000000000000000000, 0.000000000000000000, -0.000000000000000000 ) ) ;
#12691 = CYLINDRICAL_SURFACE ( 'NONE', #3142, 32.00000000000000000 ) ;
#12692 = EDGE_CURVE ( 'NONE', #10982, #12032, #18074, .T. ) ;
#12693 =( GEOMETRIC_REPRESENTATION_CONTEXT ( 3 ) GLOBAL_UNCERTAINTY_ASSIGNED_CONTEXT ( ( #12990 ) ) GLOBAL_UNIT_ASSIGNED_CONTEXT ( ( #1152, #4583, #2914 ) ) REPRESENTATION_CONTEXT ( 'NONE', 'WORKASPACE' ) );
#12694 = AXIS2_PLACEMENT_3D ( 'NONE', #3264, #1935, #18738 ) ;
#12695 = FACE_BOUND ( 'NONE', #9865, .T. ) ;
#12696 = ORIENTED_EDGE ( 'NONE', *, *, #4573, .T. ) ;
#12697 = EDGE_LOOP ( 'NONE', ( #6744, #3419, #5242, #19636 ) ) ;
#12698 = ORIENTED_EDGE ( 'NONE', *, *, #2606, .T. ) ;
#12699 = EDGE_CURVE ( 'NONE', #7569, #17874, #5028, .T. ) ;
#12700 = ORIENTED_EDGE ( 'NONE', *, *, #8783, .F. ) ;
#12701 = VERTEX_POINT ( 'NONE', #12986 ) ;
#12702 = EDGE_CURVE ( 'NONE', #16808, #2427, #19261, .T. ) ;
#12703 = DIRECTION ( 'NONE',  ( -1.000000000000000000, 0.000000000000000000, 0.000000000000000000 ) ) ;
#12704 = EDGE_LOOP ( 'NONE', ( #13129, #9512, #16425, #5080 ) ) ;
#12705 = DIRECTION ( 'NONE',  ( 0.000000000000000000, 0.000000000000000000, 1.000000000000000000 ) ) ;
#12706 = AXIS2_PLACEMENT_3D ( 'NONE', #19138, #15500, #17497 ) ;
#12707 = DIRECTION ( 'NONE',  ( 0.000000000000000000, 0.000000000000000000, -1.000000000000000000 ) ) ;
#12708 = DIRECTION ( 'NONE',  ( -1.000000000000000000, -0.000000000000000000, -0.000000000000000000 ) ) ;
#12709 = CARTESIAN_POINT ( 'NONE',  ( 10.00000000000000000, -2.208823992044743445, 85.03123271466935762 ) ) ;
#12710 = DIRECTION ( 'NONE',  ( 0.000000000000000000, 0.000000000000000000, 1.000000000000000000 ) ) ;
#12711 = DIRECTION ( 'NONE',  ( 0.000000000000000000, 0.000000000000000000, -1.000000000000000000 ) ) ;
#12712 = DIRECTION ( 'NONE',  ( -1.000000000000000000, -0.000000000000000000, 0.000000000000000000 ) ) ;
#12713 = DIRECTION ( 'NONE',  ( -1.000000000000000000, 0.000000000000000000, -0.000000000000000000 ) ) ;
#12714 = DIRECTION ( 'NONE',  ( -1.000000000000000000, 0.000000000000000000, 0.000000000000000000 ) ) ;
#12715 = EDGE_CURVE ( 'NONE', #13000, #2742, #21709, .T. ) ;
#12716 = EDGE_LOOP ( 'NONE', ( #7240, #20941, #12272, #8123 ) ) ;
#12717 = CYLINDRICAL_SURFACE ( 'NONE', #15727, 88.00000000000000000 ) ;
#12718 = CIRCLE ( 'NONE', #3201, 44.99999999999998579 ) ;
#12719 = DIRECTION ( 'NONE',  ( -1.000000000000000000, -0.000000000000000000, 0.000000000000000000 ) ) ;
#12720 = ADVANCED_FACE ( 'NONE', ( #13194 ), #9772, .F. ) ;
#12721 = CARTESIAN_POINT ( 'NONE',  ( 10.00000000000000000, 1.592605004252791279, 28.14575649959894932 ) ) ;
#12722 = ORIENTED_EDGE ( 'NONE', *, *, #4350, .T. ) ;
#12723 = DIRECTION ( 'NONE',  ( 0.000000000000000000, 0.000000000000000000, 1.000000000000000000 ) ) ;
#12724 = EDGE_LOOP ( 'NONE', ( #10711, #161, #3899, #3631 ) ) ;
#12725 = ADVANCED_FACE ( 'NONE', ( #4931 ), #19731, .F. ) ;
#12726 = ORIENTED_EDGE ( 'NONE', *, *, #1198, .F. ) ;
#12727 = DIRECTION ( 'NONE',  ( 5.760404050844383051E-17, 1.000000000000000000, -2.076472908050803616E-17 ) ) ;
#12728 = CARTESIAN_POINT ( 'NONE',  ( -7.440711023145909486, 0.000000000000000000, -104.9000000000000341 ) ) ;
#12729 = AXIS2_PLACEMENT_3D ( 'NONE', #9776, #13095, #21713 ) ;
#12730 = EDGE_LOOP ( 'NONE', ( #17465, #3360, #6802, #6786 ) ) ;
#12731 = ORIENTED_EDGE ( 'NONE', *, *, #9840, .T. ) ;
#12732 = ADVANCED_FACE ( 'NONE', ( #4597 ), #18190, .F. ) ;
#12733 = CARTESIAN_POINT ( 'NONE',  ( 10.00000000000000000, 82.02147376274727719, -42.76579056660780509 ) ) ;
#12734 = CARTESIAN_POINT ( 'NONE',  ( 10.00000000000000000, 0.000000000000000000, 0.000000000000000000 ) ) ;
#12735 = EDGE_CURVE ( 'NONE', #9557, #1558, #1274, .T. ) ;
#12736 = CYLINDRICAL_SURFACE ( 'NONE', #13233, 92.50100000000000477 ) ;
#12737 = CARTESIAN_POINT ( 'NONE',  ( 0.000000000000000000, 14.53731623274928708, 23.34226719384910709 ) ) ;
#12738 = CARTESIAN_POINT ( 'NONE',  ( 8.899999999999991473, 1.224646799147353533E-14, 100.0000000000000284 ) ) ;
#12739 = DIRECTION ( 'NONE',  ( 1.000000000000000000, 0.000000000000000000, 0.000000000000000000 ) ) ;
#12740 = CARTESIAN_POINT ( 'NONE',  ( 10.00000000000000000, 81.55207211302045778, 24.17537951050201883 ) ) ;
#12741 = DIRECTION ( 'NONE',  ( 0.000000000000000000, -0.2079116908177468248, -0.9781476007338083534 ) ) ;
#12742 = CARTESIAN_POINT ( 'NONE',  ( -10.00000000000000000, 0.000000000000000000, 0.000000000000000000 ) ) ;
#12743 = EDGE_CURVE ( 'NONE', #20936, #1592, #1285, .T. ) ;
#12744 = VERTEX_POINT ( 'NONE', #13092 ) ;
#12745 = CYLINDRICAL_SURFACE ( 'NONE', #4802, 45.00000000000000000 ) ;
#12746 = ORIENTED_EDGE ( 'NONE', *, *, #11032, .F. ) ;
#12747 = DIRECTION ( 'NONE',  ( 0.000000000000000000, 0.000000000000000000, -1.000000000000000000 ) ) ;
#12748 = VECTOR ( 'NONE', #10432, 1000.000000000000000 ) ;
#12749 = DIRECTION ( 'NONE',  ( 0.000000000000000000, 0.000000000000000000, 1.000000000000000000 ) ) ;
#12750 = ORIENTED_EDGE ( 'NONE', *, *, #11490, .T. ) ;
#12751 = FILL_AREA_STYLE ('',( #14419 ) ) ;
#12752 = ORIENTED_EDGE ( 'NONE', *, *, #690, .F. ) ;
#12753 = EDGE_LOOP ( 'NONE', ( #15779, #10309, #10384, #20973 ) ) ;
#12754 = ORIENTED_EDGE ( 'NONE', *, *, #1533, .T. ) ;
#12755 = FACE_OUTER_BOUND ( 'NONE', #7979, .T. ) ;
#12756 = CARTESIAN_POINT ( 'NONE',  ( 10.00000000000000000, -14.02138820414853448, -83.89630571862299746 ) ) ;
#12757 = ORIENTED_EDGE ( 'NONE', *, *, #10613, .T. ) ;
#12758 = CARTESIAN_POINT ( 'NONE',  ( 0.000000000000000000, 0.000000000000000000, 0.000000000000000000 ) ) ;
#12759 = FACE_OUTER_BOUND ( 'NONE', #3857, .T. ) ;
#12760 = CARTESIAN_POINT ( 'NONE',  ( 5.000000000000000000, 12.46320060045762013, -29.47318494484016327 ) ) ;
#12761 = DIRECTION ( 'NONE',  ( 0.000000000000000000, -0.4067366430757888285, -0.9135454576426059736 ) ) ;
#12762 = LINE ( 'NONE', #7477, #15079 ) ;
#12763 = VERTEX_POINT ( 'NONE', #9988 ) ;
#12764 = CARTESIAN_POINT ( 'NONE',  ( 5.000000000000002665, -24.89070495400792637, 84.40647372620493627 ) ) ;
#12765 = DIRECTION ( 'NONE',  ( -1.000000000000000000, 0.000000000000000000, 0.000000000000000000 ) ) ;
#12766 = CARTESIAN_POINT ( 'NONE',  ( 10.00000000000000000, -25.17124263951000529, -12.69364185792245081 ) ) ;
#12767 = ORIENTED_EDGE ( 'NONE', *, *, #372, .T. ) ;
#12768 = VECTOR ( 'NONE', #5568, 1000.000000000000000 ) ;
#12769 = DIRECTION ( 'NONE',  ( 1.000000000000000000, -0.000000000000000000, -0.000000000000000000 ) ) ;
#12770 = ORIENTED_EDGE ( 'NONE', *, *, #18037, .T. ) ;
#12771 = CARTESIAN_POINT ( 'NONE',  ( -10.00000000000000000, 0.000000000000000000, 0.000000000000000000 ) ) ;
#12772 = VERTEX_POINT ( 'NONE', #15074 ) ;
#12773 = DIRECTION ( 'NONE',  ( 0.000000000000000000, 0.000000000000000000, -1.000000000000000000 ) ) ;
#12774 = VERTEX_POINT ( 'NONE', #16733 ) ;
#12775 = ADVANCED_FACE ( 'NONE', ( #1604 ), #11765, .F. ) ;
#12776 = ORIENTED_EDGE ( 'NONE', *, *, #14096, .F. ) ;
#12777 = CARTESIAN_POINT ( 'NONE',  ( 0.000000000000000000, -28.00896854772002342, 15.47571261340914539 ) ) ;
#12778 = VERTEX_POINT ( 'NONE', #4697 ) ;
#12779 = DIRECTION ( 'NONE',  ( -1.000000000000000000, -0.000000000000000000, -0.000000000000000000 ) ) ;
#12780 = CIRCLE ( 'NONE', #16672, 12.00000000000000000 ) ;
#12781 = CARTESIAN_POINT ( 'NONE',  ( 5.000000000000000000, 75.87763420127893710, -44.57111876559645225 ) ) ;
#12782 = CARTESIAN_POINT ( 'NONE',  ( 1.129531546211711479, 0.000000000000000000, 0.000000000000000000 ) ) ;
#12783 = DIRECTION ( 'NONE',  ( -1.000000000000000000, 0.000000000000000000, 0.000000000000000000 ) ) ;
#12784 = ADVANCED_FACE ( 'NONE', ( #384 ), #12201, .F. ) ;
#12785 = CARTESIAN_POINT ( 'NONE',  ( 10.00000000000000000, -14.53731623274945406, 23.34226719384900761 ) ) ;
#12786 = DIRECTION ( 'NONE',  ( -1.000000000000000000, -0.000000000000000000, -0.000000000000000000 ) ) ;
#12787 = AXIS2_PLACEMENT_3D ( 'NONE', #20627, #15646, #10464 ) ;
#12788 = CYLINDRICAL_SURFACE ( 'NONE', #14365, 6.887500000000022382 ) ;
#12789 = DIRECTION ( 'NONE',  ( 0.000000000000000000, 0.000000000000000000, -1.000000000000000000 ) ) ;
#12790 = CIRCLE ( 'NONE', #1165, 88.00000000000000000 ) ;
#12791 = DIRECTION ( 'NONE',  ( 0.000000000000000000, 0.000000000000000000, -1.000000000000000000 ) ) ;
#12792 = VERTEX_POINT ( 'NONE', #18732 ) ;
#12793 = AXIS2_PLACEMENT_3D ( 'NONE', #1987, #20867, #7400 ) ;
#12794 = ORIENTED_EDGE ( 'NONE', *, *, #3290, .F. ) ;
#12795 = ORIENTED_EDGE ( 'NONE', *, *, #16707, .T. ) ;
#12796 = CIRCLE ( 'NONE', #13499, 11.99999999999999822 ) ;
#12797 = CIRCLE ( 'NONE', #10643, 27.49900000000000233 ) ;
#12798 = ORIENTED_EDGE ( 'NONE', *, *, #8665, .F. ) ;
#12799 = EDGE_CURVE ( 'NONE', #16358, #12017, #6572, .T. ) ;
#12800 = AXIS2_PLACEMENT_3D ( 'NONE', #8223, #8126, #15066 ) ;
#12801 = ORIENTED_EDGE ( 'NONE', *, *, #2437, .T. ) ;
#12802 = CARTESIAN_POINT ( 'NONE',  ( 10.00000000000000000, 0.000000000000000000, 0.000000000000000000 ) ) ;
#12803 = ORIENTED_EDGE ( 'NONE', *, *, #9355, .F. ) ;
#12804 = FACE_OUTER_BOUND ( 'NONE', #8539, .T. ) ;
#12805 = CARTESIAN_POINT ( 'NONE',  ( 0.000000000000000000, 0.000000000000000000, 0.000000000000000000 ) ) ;
#12806 = DIRECTION ( 'NONE',  ( -1.000000000000000000, -0.000000000000000000, 0.000000000000000000 ) ) ;
#12807 = CIRCLE ( 'NONE', #6133, 12.00000000000000000 ) ;
#12808 = DIRECTION ( 'NONE',  ( -1.000000000000000000, -0.000000000000000000, -0.000000000000000000 ) ) ;
#12809 = CYLINDRICAL_SURFACE ( 'NONE', #7865, 44.99999999999999289 ) ;
#12810 = LINE ( 'NONE', #19558, #13280 ) ;
#12811 = CARTESIAN_POINT ( 'NONE',  ( 10.00000000000000000, 67.05625154133453236, 63.71729851637834940 ) ) ;
#12812 = DIRECTION ( 'NONE',  ( -1.000000000000000000, -0.000000000000000000, -0.000000000000000000 ) ) ;
#12813 = EDGE_CURVE ( 'NONE', #9285, #19310, #7611, .T. ) ;
#12814 = CARTESIAN_POINT ( 'NONE',  ( 10.00000000000000000, 0.000000000000000000, 0.000000000000000000 ) ) ;
#12815 = AXIS2_PLACEMENT_3D ( 'NONE', #7125, #6809, #3371 ) ;
#12816 = ORIENTED_EDGE ( 'NONE', *, *, #13405, .F. ) ;
#12817 = CIRCLE ( 'NONE', #10000, 11.99999999999999822 ) ;
#12818 = EDGE_CURVE ( 'NONE', #12527, #17019, #13614, .T. ) ;
#12819 = FACE_OUTER_BOUND ( 'NONE', #19218, .T. ) ;
#12820 = AXIS2_PLACEMENT_3D ( 'NONE', #18482, #14940, #19918 ) ;
#12821 = VERTEX_POINT ( 'NONE', #15186 ) ;
#12822 = LINE ( 'NONE', #19572, #10174 ) ;
#12823 = CARTESIAN_POINT ( 'NONE',  ( 10.00000000000000000, 0.000000000000000000, 0.000000000000000000 ) ) ;
#12824 = CIRCLE ( 'NONE', #1546, 114.9007999999999896 ) ;
#12825 = EDGE_CURVE ( 'NONE', #12425, #17806, #15018, .T. ) ;
#12826 = ORIENTED_EDGE ( 'NONE', *, *, #15165, .F. ) ;
#12827 = EDGE_CURVE ( 'NONE', #11727, #659, #8669, .T. ) ;
#12828 = EDGE_CURVE ( 'NONE', #12830, #12032, #6215, .T. ) ;
#12829 = LINE ( 'NONE', #7335, #15357 ) ;
#12830 = VERTEX_POINT ( 'NONE', #12085 ) ;
#12831 = ORIENTED_EDGE ( 'NONE', *, *, #2179, .T. ) ;
#12832 = PRODUCT_CONTEXT ( 'NONE', #14335, 'mechanical' ) ;
#12833 = DIRECTION ( 'NONE',  ( 1.000000000000000000, 0.000000000000000000, 0.000000000000000000 ) ) ;
#12834 = EDGE_CURVE ( 'NONE', #2240, #16026, #14673, .T. ) ;
#12835 = ORIENTED_EDGE ( 'NONE', *, *, #2470, .F. ) ;
#12836 = ORIENTED_EDGE ( 'NONE', *, *, #16538, .T. ) ;
#12837 = DIRECTION ( 'NONE',  ( -0.000000000000000000, -0.000000000000000000, -1.000000000000000000 ) ) ;
#12838 = AXIS2_PLACEMENT_3D ( 'NONE', #20273, #1818, #11870 ) ;
#12839 = LINE ( 'NONE', #14508, #4560 ) ;
#12840 = DIRECTION ( 'NONE',  ( 0.000000000000000000, -0.9510565162951565288, 0.3090169943749382919 ) ) ;
#12841 = LINE ( 'NONE', #20916, #12623 ) ;
#12842 = DIRECTION ( 'NONE',  ( 1.000000000000000000, 0.000000000000000000, 0.000000000000000000 ) ) ;
#12843 = CARTESIAN_POINT ( 'NONE',  ( 0.000000000000000000, 66.01871308925549897, -64.79170103522952218 ) ) ;
#12844 = FACE_BOUND ( 'NONE', #6419, .T. ) ;
#12845 = DIRECTION ( 'NONE',  ( -1.000000000000000000, -0.000000000000000000, -0.000000000000000000 ) ) ;
#12846 = EDGE_CURVE ( 'NONE', #2607, #18262, #4790, .T. ) ;
#12847 = DIRECTION ( 'NONE',  ( 0.000000000000000000, -0.4067366430757888285, -0.9135454576426059736 ) ) ;
#12848 = CIRCLE ( 'NONE', #9651, 45.00000000000000711 ) ;
#12849 = ORIENTED_EDGE ( 'NONE', *, *, #3928, .F. ) ;
#12850 = EDGE_CURVE ( 'NONE', #1024, #17734, #17850, .T. ) ;
#12851 = EDGE_CURVE ( 'NONE', #1865, #17490, #19960, .T. ) ;
#12852 = CARTESIAN_POINT ( 'NONE',  ( 0.000000000000000000, -86.66425444033941972, 32.33793443156368141 ) ) ;
#12853 = VECTOR ( 'NONE', #21058, 1000.000000000000000 ) ;
#12854 = ORIENTED_EDGE ( 'NONE', *, *, #19492, .T. ) ;
#12855 = CIRCLE ( 'NONE', #20971, 6.728125000000023448 ) ;
#12856 = EDGE_CURVE ( 'NONE', #15286, #12492, #17181, .T. ) ;
#12857 = CARTESIAN_POINT ( 'NONE',  ( 0.000000000000000000, 8.134922360106093819, 84.67002113262482510 ) ) ;
#12858 = LINE ( 'NONE', #8446, #10224 ) ;
#12859 = CYLINDRICAL_SURFACE ( 'NONE', #20457, 32.00000000000000000 ) ;
#12860 = ORIENTED_EDGE ( 'NONE', *, *, #18514, .F. ) ;
#12861 =( NAMED_UNIT ( * ) PLANE_ANGLE_UNIT ( ) SI_UNIT ( $, .RADIAN. ) );
#12862 = ORIENTED_EDGE ( 'NONE', *, *, #8007, .F. ) ;
#12863 = EDGE_CURVE ( 'NONE', #21566, #18952, #8778, .T. ) ;
#12864 = VERTEX_POINT ( 'NONE', #13967 ) ;
#12865 = CONICAL_SURFACE ( 'NONE', #6183, 5.612499999999999822, 0.4883339510564123076 ) ;
#12866 = ORIENTED_EDGE ( 'NONE', *, *, #8685, .T. ) ;
#12867 = CYLINDRICAL_SURFACE ( 'NONE', #5786, 44.99999999999998579 ) ;
#12868 = DIRECTION ( 'NONE',  ( 0.000000000000000000, 0.000000000000000000, -1.000000000000000000 ) ) ;
#12869 = ORIENTED_EDGE ( 'NONE', *, *, #8090, .T. ) ;
#12870 = CIRCLE ( 'NONE', #20689, 104.9000000000000341 ) ;
#12871 = EDGE_CURVE ( 'NONE', #21761, #13692, #13962, .T. ) ;
#12872 = DIRECTION ( 'NONE',  ( 0.000000000000000000, 0.000000000000000000, 1.000000000000000000 ) ) ;
#12873 = DIRECTION ( 'NONE',  ( 1.000000000000000000, 0.000000000000000000, 0.000000000000000000 ) ) ;
#12874 = CYLINDRICAL_SURFACE ( 'NONE', #15003, 7.500000000000000000 ) ;
#12875 = CARTESIAN_POINT ( 'NONE',  ( 0.000000000000000000, 0.000000000000000000, 0.000000000000000000 ) ) ;
#12876 = AXIS2_PLACEMENT_3D ( 'NONE', #4955, #6620, #21299 ) ;
#12877 = DIRECTION ( 'NONE',  ( 0.000000000000000000, 0.000000000000000000, 1.000000000000000000 ) ) ;
#12878 = ORIENTED_EDGE ( 'NONE', *, *, #6670, .T. ) ;
#12879 = EDGE_CURVE ( 'NONE', #19613, #13415, #6931, .T. ) ;
#12880 = DIRECTION ( 'NONE',  ( 1.000000000000000000, -0.000000000000000000, -0.000000000000000000 ) ) ;
#12881 = CARTESIAN_POINT ( 'NONE',  ( 10.00000000000000000, 30.61448696004452330, 9.314139153634327428 ) ) ;
#12882 = ORIENTED_EDGE ( 'NONE', *, *, #12217, .T. ) ;
#12883 = AXIS2_PLACEMENT_3D ( 'NONE', #17220, #3517, #8816 ) ;
#12884 = AXIS2_PLACEMENT_3D ( 'NONE', #151, #16953, #1808 ) ;
#12885 = CIRCLE ( 'NONE', #12176, 44.99999999999999289 ) ;
#12886 = EDGE_CURVE ( 'NONE', #1075, #15764, #898, .T. ) ;
#12887 = DIRECTION ( 'NONE',  ( 1.000000000000000000, 0.000000000000000000, 0.000000000000000000 ) ) ;
#12888 = CIRCLE ( 'NONE', #19232, 12.00000000000000000 ) ;
#12889 = ORIENTED_EDGE ( 'NONE', *, *, #5006, .T. ) ;
#12890 = CARTESIAN_POINT ( 'NONE',  ( 0.000000000000000000, -13.56333590714035253, 28.98337314858430602 ) ) ;
#12891 = CARTESIAN_POINT ( 'NONE',  ( 0.000000000000000000, 71.33759994382042180, -58.88447872958914786 ) ) ;
#12892 = ORIENTED_EDGE ( 'NONE', *, *, #12022, .T. ) ;
#12893 = CARTESIAN_POINT ( 'NONE',  ( 5.000000000000002665, -87.92084725184945171, -3.731570516143874361 ) ) ;
#12894 = ORIENTED_EDGE ( 'NONE', *, *, #18928, .F. ) ;
#12895 = ORIENTED_EDGE ( 'NONE', *, *, #14488, .F. ) ;
#12896 = CIRCLE ( 'NONE', #18560, 11.99999999999999822 ) ;
#12897 = FACE_OUTER_BOUND ( 'NONE', #4480, .T. ) ;
#12898 = ORIENTED_EDGE ( 'NONE', *, *, #19488, .T. ) ;
#12899 = CYLINDRICAL_SURFACE ( 'NONE', #5972, 27.49900000000000233 ) ;
#12900 = CARTESIAN_POINT ( 'NONE',  ( 10.00000000000000000, -16.79755869217588682, -90.96305306542271296 ) ) ;
#12901 = CARTESIAN_POINT ( 'NONE',  ( 0.000000000000000000, 0.000000000000000000, 0.000000000000000000 ) ) ;
#12902 = VECTOR ( 'NONE', #18698, 1000.000000000000000 ) ;
#12903 = VECTOR ( 'NONE', #15740, 1000.000000000000000 ) ;
#12904 = DIRECTION ( 'NONE',  ( 0.000000000000000000, -0.9848077530122096857, 0.1736481776669207000 ) ) ;
#12905 = VECTOR ( 'NONE', #21600, 1000.000000000000000 ) ;
#12906 = AXIS2_PLACEMENT_3D ( 'NONE', #15820, #15708, #7210 ) ;
#12907 = DIRECTION ( 'NONE',  ( 0.000000000000000000, -0.9510565162951565288, 0.3090169943749382919 ) ) ;
#12908 = DIRECTION ( 'NONE',  ( 0.000000000000000000, 0.7431448254773910245, 0.6691306063588617903 ) ) ;
#12909 = DIRECTION ( 'NONE',  ( 1.000000000000000000, 0.000000000000000000, 0.000000000000000000 ) ) ;
#12910 = DIRECTION ( 'NONE',  ( 0.000000000000000000, 0.000000000000000000, 1.000000000000000000 ) ) ;
#12911 = DIRECTION ( 'NONE',  ( 0.000000000000000000, -0.9945218953682722907, -0.1045284632676635739 ) ) ;
#12912 = CIRCLE ( 'NONE', #7986, 88.00000000000000000 ) ;
#12913 = ORIENTED_EDGE ( 'NONE', *, *, #11942, .F. ) ;
#12914 = AXIS2_PLACEMENT_3D ( 'NONE', #6658, #17020, #18792 ) ;
#12915 = ORIENTED_EDGE ( 'NONE', *, *, #6971, .F. ) ;
#12916 = VECTOR ( 'NONE', #3564, 1000.000000000000000 ) ;
#12917 = ORIENTED_EDGE ( 'NONE', *, *, #20119, .T. ) ;
#12918 = ORIENTED_EDGE ( 'NONE', *, *, #15653, .T. ) ;
#12919 = ORIENTED_EDGE ( 'NONE', *, *, #14582, .F. ) ;
#12920 = CARTESIAN_POINT ( 'NONE',  ( 0.000000000000000000, -90.32141448704695108, 19.96189084378192291 ) ) ;
#12921 = EDGE_LOOP ( 'NONE', ( #4708, #533, #8231, #19384 ) ) ;
#12922 = DIRECTION ( 'NONE',  ( 0.000000000000000000, 0.000000000000000000, -1.000000000000000000 ) ) ;
#12923 = CARTESIAN_POINT ( 'NONE',  ( -2.799999999999996714, 60.00000000000000000, 9.999999999999998224 ) ) ;
#12924 = CARTESIAN_POINT ( 'NONE',  ( 0.000000000000000000, -75.87763420127802760, -44.57111876559801544 ) ) ;
#12925 = CARTESIAN_POINT ( 'NONE',  ( 10.00000000000000000, 2.481790431840499966, -92.46770094066590673 ) ) ;
#12926 = CARTESIAN_POINT ( 'NONE',  ( 0.000000000000000000, 0.000000000000000000, 5.000000000000004441 ) ) ;
#12927 = AXIS2_PLACEMENT_3D ( 'NONE', #9068, #15819, #4106 ) ;
#12928 = DIRECTION ( 'NONE',  ( -1.000000000000000000, -0.000000000000000000, 0.000000000000000000 ) ) ;
#12929 = CYLINDRICAL_SURFACE ( 'NONE', #2005, 92.50100000000000477 ) ;
#12930 = CARTESIAN_POINT ( 'NONE',  ( 0.000000000000000000, 3.786343810537573074, 27.23708136986053674 ) ) ;
#12931 = ADVANCED_FACE ( 'NONE', ( #15615 ), #7232, .F. ) ;
#12932 = VERTEX_POINT ( 'NONE', #19054 ) ;
#12933 = CARTESIAN_POINT ( 'NONE',  ( 10.00000000000000000, -84.90234713953981327, -5.175025661884713912 ) ) ;
#12934 = ORIENTED_EDGE ( 'NONE', *, *, #7988, .T. ) ;
#12935 = EDGE_CURVE ( 'NONE', #4602, #6281, #7271, .T. ) ;
#12936 = LINE ( 'NONE', #4658, #1710 ) ;
#12937 = AXIS2_PLACEMENT_3D ( 'NONE', #21555, #14700, #3101 ) ;
#12938 = DIRECTION ( 'NONE',  ( 0.000000000000000000, 0.000000000000000000, -1.000000000000000000 ) ) ;
#12939 = ORIENTED_EDGE ( 'NONE', *, *, #7050, .F. ) ;
#12940 = AXIS2_PLACEMENT_3D ( 'NONE', #19515, #12555, #743 ) ;
#12941 = DIRECTION ( 'NONE',  ( 1.000000000000000000, 0.000000000000000000, 0.000000000000000000 ) ) ;
#12942 = ORIENTED_EDGE ( 'NONE', *, *, #8486, .F. ) ;
#12943 = EDGE_LOOP ( 'NONE', ( #14137, #17879, #16959, #17992 ) ) ;
#12944 = DIRECTION ( 'NONE',  ( 0.000000000000000000, 0.000000000000000000, 1.000000000000000000 ) ) ;
#12945 = EDGE_CURVE ( 'NONE', #21410, #21168, #19611, .T. ) ;
#12946 = CARTESIAN_POINT ( 'NONE',  ( 10.00000000000000000, 25.56104204395304080, 81.12843256239672485 ) ) ;
#12947 = ORIENTED_EDGE ( 'NONE', *, *, #17184, .T. ) ;
#12948 = ORIENTED_EDGE ( 'NONE', *, *, #16182, .T. ) ;
#12949 = CARTESIAN_POINT ( 'NONE',  ( 10.00000000000000000, 86.54587337002898551, -15.93147207946920396 ) ) ;
#12950 = CARTESIAN_POINT ( 'NONE',  ( 10.00000000000000000, -92.22057093985026199, -7.197311757041478408 ) ) ;
#12951 = CARTESIAN_POINT ( 'NONE',  ( 10.00000000000000000, -15.51843147776295950, -83.63233659819665888 ) ) ;
#12952 = DIRECTION ( 'NONE',  ( 1.000000000000000000, 0.000000000000000000, 0.000000000000000000 ) ) ;
#12953 = DIRECTION ( 'NONE',  ( 1.000000000000000000, 0.000000000000000000, 0.000000000000000000 ) ) ;
#12954 = DIRECTION ( 'NONE',  ( 0.000000000000000000, 0.000000000000000000, 1.000000000000000000 ) ) ;
#12955 = LINE ( 'NONE', #18276, #10709 ) ;
#12956 = FACE_OUTER_BOUND ( 'NONE', #15413, .T. ) ;
#12957 = DIRECTION ( 'NONE',  ( 0.000000000000000000, 1.773272886554069860E-14, -1.000000000000000000 ) ) ;
#12958 = AXIS2_PLACEMENT_3D ( 'NONE', #1315, #8061, #19655 ) ;
#12959 = ADVANCED_FACE ( 'NONE', ( #7550 ), #20919, .F. ) ;
#12960 = ADVANCED_FACE ( 'NONE', ( #1036 ), #12627, .F. ) ;
#12961 = VECTOR ( 'NONE', #9315, 1000.000000000000114 ) ;
#12962 = ADVANCED_FACE ( 'NONE', ( #4242 ), #8980, .F. ) ;
#12963 = ORIENTED_EDGE ( 'NONE', *, *, #9509, .F. ) ;
#12964 = AXIS2_PLACEMENT_3D ( 'NONE', #16991, #8590, #13341 ) ;
#12965 = AXIS2_PLACEMENT_3D ( 'NONE', #19297, #11227, #16414 ) ;
#12966 = EDGE_CURVE ( 'NONE', #12565, #4587, #17506, .T. ) ;
#12967 = VERTEX_POINT ( 'NONE', #5902 ) ;
#12968 = CARTESIAN_POINT ( 'NONE',  ( -8.000000000000007105, 0.000000000000000000, -115.1000000000000227 ) ) ;
#12969 = LINE ( 'NONE', #14850, #5993 ) ;
#12970 = ORIENTED_EDGE ( 'NONE', *, *, #1784, .F. ) ;
#12971 =( NAMED_UNIT ( * ) PLANE_ANGLE_UNIT ( ) SI_UNIT ( $, .RADIAN. ) );
#12972 = EDGE_CURVE ( 'NONE', #52, #12455, #19266, .T. ) ;
#12973 = CIRCLE ( 'NONE', #18982, 88.00000000000000000 ) ;
#12974 = ORIENTED_EDGE ( 'NONE', *, *, #1587, .F. ) ;
#12975 = ORIENTED_EDGE ( 'NONE', *, *, #15248, .F. ) ;
#12976 = AXIS2_PLACEMENT_3D ( 'NONE', #19250, #16151, #5665 ) ;
#12977 = EDGE_LOOP ( 'NONE', ( #8656, #13985, #12392, #18615 ) ) ;
#12978 = AXIS2_PLACEMENT_3D ( 'NONE', #11222, #6266, #15967 ) ;
#12979 = DIRECTION ( 'NONE',  ( -1.000000000000000000, 0.000000000000000000, 0.000000000000000000 ) ) ;
#12980 = DIRECTION ( 'NONE',  ( 1.000000000000000000, -0.000000000000000000, 0.000000000000000000 ) ) ;
#12981 = AXIS2_PLACEMENT_3D ( 'NONE', #10197, #8538, #2226 ) ;
#12982 = ORIENTED_EDGE ( 'NONE', *, *, #15695, .T. ) ;
#12983 = EDGE_CURVE ( 'NONE', #2019, #12158, #20333, .T. ) ;
#12984 = CARTESIAN_POINT ( 'NONE',  ( 10.00000000000000000, -83.03980459022467642, -18.42770452393328995 ) ) ;
#12985 = CARTESIAN_POINT ( 'NONE',  ( 10.00000000000000000, 4.000000000000000000, 0.000000000000000000 ) ) ;
#12986 = CARTESIAN_POINT ( 'NONE',  ( 7.500000000000000000, 9.184850993605147944E-16, 3.000000000000000000 ) ) ;
#12987 = CARTESIAN_POINT ( 'NONE',  ( 10.00000000000000000, 23.10190250628834718, 89.56973317806607326 ) ) ;
#12988 = AXIS2_PLACEMENT_3D ( 'NONE', #11847, #15487, #16941 ) ;
#12989 = CARTESIAN_POINT ( 'NONE',  ( 0.000000000000000000, -12.94633825542249994, -24.26081875733348170 ) ) ;
#12990 = UNCERTAINTY_MEASURE_WITH_UNIT (LENGTH_MEASURE( 1.000000000000000082E-05 ), #1152, 'distance_accuracy_value', 'NONE');
#12991 = ORIENTED_EDGE ( 'NONE', *, *, #9687, .F. ) ;
#12992 = DIRECTION ( 'NONE',  ( 0.000000000000000000, 0.000000000000000000, 1.000000000000000000 ) ) ;
#12993 = CIRCLE ( 'NONE', #15823, 44.99999999999999289 ) ;
#12994 = EDGE_CURVE ( 'NONE', #11658, #21836, #11488, .T. ) ;
#12995 = FACE_OUTER_BOUND ( 'NONE', #9978, .T. ) ;
#12996 = ORIENTED_EDGE ( 'NONE', *, *, #14507, .T. ) ;
#12997 = CIRCLE ( 'NONE', #21816, 5.000000000000000000 ) ;
#12998 = AXIS2_PLACEMENT_3D ( 'NONE', #12603, #19352, #6000 ) ;
#12999 = FACE_OUTER_BOUND ( 'NONE', #8721, .T. ) ;
#13000 = VERTEX_POINT ( 'NONE', #12405 ) ;
#13001 = CARTESIAN_POINT ( 'NONE',  ( 0.000000000000000000, 9.646732466565339337, 84.51112348751853176 ) ) ;
#13002 = DIRECTION ( 'NONE',  ( 1.000000000000000000, 0.000000000000000000, 0.000000000000000000 ) ) ;
#13003 = ORIENTED_EDGE ( 'NONE', *, *, #14067, .T. ) ;
#13004 = CARTESIAN_POINT ( 'NONE',  ( 1.500000000000001332, 0.000000000000000000, 0.000000000000000000 ) ) ;
#13005 = ADVANCED_FACE ( 'NONE', ( #7664 ), #2473, .F. ) ;
#13006 = VERTEX_POINT ( 'NONE', #4131 ) ;
#13007 = VERTEX_POINT ( 'NONE', #12738 ) ;
#13008 = DIRECTION ( 'NONE',  ( 1.000000000000000000, 0.000000000000000000, -0.000000000000000000 ) ) ;
#13009 = EDGE_CURVE ( 'NONE', #18240, #11426, #233, .T. ) ;
#13010 = ORIENTED_EDGE ( 'NONE', *, *, #10560, .F. ) ;
#13011 = DIRECTION ( 'NONE',  ( -1.000000000000000000, -0.000000000000000000, -0.000000000000000000 ) ) ;
#13012 = VECTOR ( 'NONE', #11248, 1000.000000000000000 ) ;
#13013 = CARTESIAN_POINT ( 'NONE',  ( -90.00000000000000000, 1.469576158976824302E-14, 120.0000000000000426 ) ) ;
#13014 = CARTESIAN_POINT ( 'NONE',  ( 0.000000000000000000, 17.83210509884640871, 21.83428559348767806 ) ) ;
#13015 = CIRCLE ( 'NONE', #9484, 92.50100000000000477 ) ;
#13016 = EDGE_CURVE ( 'NONE', #6398, #14549, #6949, .T. ) ;
#13017 = TOROIDAL_SURFACE ( 'NONE', #16184, 105.0992000000000104, 0.2042000000000007420 ) ;
#13018 = PRODUCT ( 'radial cylindrical roller bearing_iso_ISO 15 RCR - 17200 - 54,SI,NC,54', 'radial cylindrical roller bearing_iso_ISO 15 RCR - 17200 - 54,SI,NC,54', '', ( #19582 ) ) ;
#13019 = DIRECTION ( 'NONE',  ( -1.000000000000000000, 0.000000000000000000, -0.000000000000000000 ) ) ;
#13020 = EDGE_CURVE ( 'NONE', #6719, #20752, #17156, .T. ) ;
#13021 = CARTESIAN_POINT ( 'NONE',  ( 10.00000000000000000, 81.32027326007924728, -44.08455690948972716 ) ) ;
#13022 = DIRECTION ( 'NONE',  ( -1.000000000000000000, -0.000000000000000000, 0.000000000000000000 ) ) ;
#13023 = CARTESIAN_POINT ( 'NONE',  ( 0.000000000000000000, -46.07110168784872428, 74.97635353408365688 ) ) ;
#13024 = DIRECTION ( 'NONE',  ( 0.000000000000000000, 0.9848077530122085754, -0.1736481776669273613 ) ) ;
#13025 = CYLINDRICAL_SURFACE ( 'NONE', #1232, 32.00000000000000000 ) ;
#13026 = DIRECTION ( 'NONE',  ( 1.000000000000000000, 0.000000000000000000, 0.000000000000000000 ) ) ;
#13027 = AXIS2_PLACEMENT_3D ( 'NONE', #19857, #13011, #21734 ) ;
#13028 = ORIENTED_EDGE ( 'NONE', *, *, #12886, .F. ) ;
#13029 = AXIS2_PLACEMENT_3D ( 'NONE', #5695, #18643, #3497 ) ;
#13030 = ORIENTED_EDGE ( 'NONE', *, *, #20691, .F. ) ;
#13031 = AXIS2_PLACEMENT_3D ( 'NONE', #3496, #20184, #10232 ) ;
#13032 = AXIS2_PLACEMENT_3D ( 'NONE', #6842, #10466, #17218 ) ;
#13033 = VERTEX_POINT ( 'NONE', #9197 ) ;
#13034 = ORIENTED_EDGE ( 'NONE', *, *, #20412, .F. ) ;
#13035 = EDGE_LOOP ( 'NONE', ( #11618, #20348, #2501, #14905 ) ) ;
#13036 = DIRECTION ( 'NONE',  ( 0.000000000000000000, -0.3420201433256756518, 0.9396926207859059854 ) ) ;
#13037 = ORIENTED_EDGE ( 'NONE', *, *, #15864, .F. ) ;
#13038 = DIRECTION ( 'NONE',  ( -1.000000000000000000, 0.000000000000000000, -0.000000000000000000 ) ) ;
#13039 = CARTESIAN_POINT ( 'NONE',  ( 0.000000000000000000, 7.240962358591984227, -31.16999300804307538 ) ) ;
#13040 = LINE ( 'NONE', #2983, #11388 ) ;
#13041 = CARTESIAN_POINT ( 'NONE',  ( 10.00000000000000000, -87.58454185039444440, 8.540961822681374827 ) ) ;
#13042 = FACE_OUTER_BOUND ( 'NONE', #10465, .T. ) ;
#13043 = AXIS2_PLACEMENT_3D ( 'NONE', #6487, #21180, #12992 ) ;
#13044 = CARTESIAN_POINT ( 'NONE',  ( 0.000000000000000000, 14.02138820415029663, -83.89630571862271324 ) ) ;
#13045 = CARTESIAN_POINT ( 'NONE',  ( 0.000000000000000000, -6.797690662955810481, 87.73705831432212676 ) ) ;
#13046 = ORIENTED_EDGE ( 'NONE', *, *, #8818, .T. ) ;
#13047 = DIRECTION ( 'NONE',  ( 1.000000000000000000, 0.000000000000000000, 0.000000000000000000 ) ) ;
#13048 = ORIENTED_EDGE ( 'NONE', *, *, #21029, .T. ) ;
#13049 = VERTEX_POINT ( 'NONE', #14511 ) ;
#13050 = CARTESIAN_POINT ( 'NONE',  ( 5.000000000000002665, 23.62010150527222052, 84.77081340225913664 ) ) ;
#13051 = DIRECTION ( 'NONE',  ( 1.000000000000000000, 0.000000000000000000, 0.000000000000000000 ) ) ;
#13052 = VERTEX_POINT ( 'NONE', #14076 ) ;
#13053 = CIRCLE ( 'NONE', #714, 44.99999999999999289 ) ;
#13054 = CARTESIAN_POINT ( 'NONE',  ( 0.000000000000000000, 69.25892805976580746, -49.38005998797770246 ) ) ;
#13055 = ORIENTED_EDGE ( 'NONE', *, *, #7423, .F. ) ;
#13056 = ORIENTED_EDGE ( 'NONE', *, *, #20504, .F. ) ;
#13057 = DIRECTION ( 'NONE',  ( -2.140611735271808086E-17, -1.000000000000000000, -4.506460675456328835E-17 ) ) ;
#13058 = DIRECTION ( 'NONE',  ( 0.000000000000000000, 0.000000000000000000, -1.000000000000000000 ) ) ;
#13059 = ORIENTED_EDGE ( 'NONE', *, *, #18023, .T. ) ;
#13060 = EDGE_CURVE ( 'NONE', #8089, #16217, #19276, .T. ) ;
#13061 = ORIENTED_EDGE ( 'NONE', *, *, #3958, .F. ) ;
#13062 = DIRECTION ( 'NONE',  ( 1.000000000000000000, 0.000000000000000000, 0.000000000000000000 ) ) ;
#13063 = DIRECTION ( 'NONE',  ( 1.000000000000000000, 0.000000000000000000, 0.000000000000000000 ) ) ;
#13064 = DIRECTION ( 'NONE',  ( 0.000000000000000000, 0.000000000000000000, 1.000000000000000000 ) ) ;
#13065 = CARTESIAN_POINT ( 'NONE',  ( 5.000000000000002665, 0.6609040254611577847, 87.99751818016873983 ) ) ;
#13066 = CARTESIAN_POINT ( 'NONE',  ( 10.00000000000000000, -69.74988376404053270, 53.65588238863315240 ) ) ;
#13067 = DIRECTION ( 'NONE',  ( 0.000000000000000000, 0.000000000000000000, -1.000000000000000000 ) ) ;
#13068 = EDGE_CURVE ( 'NONE', #13441, #7892, #15034, .T. ) ;
#13069 = CARTESIAN_POINT ( 'NONE',  ( 10.00000000000000000, 0.000000000000000000, 0.000000000000000000 ) ) ;
#13070 = DIRECTION ( 'NONE',  ( 0.000000000000000000, 0.000000000000000000, 1.000000000000000000 ) ) ;
#13071 = CARTESIAN_POINT ( 'NONE',  ( 5.000000000000000000, 52.25832601289098278, 70.80301803122803506 ) ) ;
#13072 = CIRCLE ( 'NONE', #13791, 92.50099999999999056 ) ;
#13073 = ORIENTED_EDGE ( 'NONE', *, *, #808, .F. ) ;
#13074 = EDGE_LOOP ( 'NONE', ( #15335, #953, #8190, #20836 ) ) ;
#13075 = CARTESIAN_POINT ( 'NONE',  ( 10.00000000000000000, -56.05743251323904985, 67.83483072893783117 ) ) ;
#13076 = DIRECTION ( 'NONE',  ( 0.000000000000000000, 0.6427876096865403621, -0.7660444431189772363 ) ) ;
#13077 = DIRECTION ( 'NONE',  ( 0.000000000000000000, 0.4694715627858855322, 0.8829475928589297640 ) ) ;
#13078 = ORIENTED_EDGE ( 'NONE', *, *, #9760, .T. ) ;
#13079 = PRESENTATION_STYLE_ASSIGNMENT (( #7898 ) ) ;
#13080 = ORIENTED_EDGE ( 'NONE', *, *, #13855, .T. ) ;
#13081 = VERTEX_POINT ( 'NONE', #20819 ) ;
#13082 = EDGE_CURVE ( 'NONE', #239, #1840, #6583, .T. ) ;
#13083 = EDGE_CURVE ( 'NONE', #2596, #17874, #7286, .T. ) ;
#13084 = ORIENTED_EDGE ( 'NONE', *, *, #17037, .F. ) ;
#13085 =( GEOMETRIC_REPRESENTATION_CONTEXT ( 3 ) GLOBAL_UNCERTAINTY_ASSIGNED_CONTEXT ( ( #8140 ) ) GLOBAL_UNIT_ASSIGNED_CONTEXT ( ( #15750, #3711, #19283 ) ) REPRESENTATION_CONTEXT ( 'NONE', 'WORKASPACE' ) );
#13086 = CARTESIAN_POINT ( 'NONE',  ( 0.000000000000000000, 15.25521607131206459, 23.70650506194175478 ) ) ;
#13087 = FACE_OUTER_BOUND ( 'NONE', #2764, .T. ) ;
#13088 = MANIFOLD_SOLID_BREP ( 'Keyway', #15352 ) ;
#13089 = ORIENTED_EDGE ( 'NONE', *, *, #1521, .T. ) ;
#13090 = CARTESIAN_POINT ( 'NONE',  ( 0.000000000000000000, 0.000000000000000000, 0.000000000000000000 ) ) ;
#13091 = FACE_OUTER_BOUND ( 'NONE', #15281, .T. ) ;
#13092 = CARTESIAN_POINT ( 'NONE',  ( 10.00000000000000000, 3.786343810537937227, -27.23708136986048700 ) ) ;
#13093 = DIRECTION ( 'NONE',  ( -1.000000000000000000, -0.000000000000000000, -0.000000000000000000 ) ) ;
#13094 = DIRECTION ( 'NONE',  ( -1.000000000000000000, 0.000000000000000000, -0.000000000000000000 ) ) ;
#13095 = DIRECTION ( 'NONE',  ( 1.000000000000000000, 0.000000000000000000, 0.000000000000000000 ) ) ;
#13096 = ORIENTED_EDGE ( 'NONE', *, *, #13345, .F. ) ;
#13097 = DIRECTION ( 'NONE',  ( 0.000000000000000000, 0.1391731009600591373, 0.9902680687415712502 ) ) ;
#13098 = EDGE_CURVE ( 'NONE', #19754, #3874, #3744, .T. ) ;
#13099 = DIRECTION ( 'NONE',  ( 1.000000000000000000, 0.000000000000000000, 0.000000000000000000 ) ) ;
#13100 = ORIENTED_EDGE ( 'NONE', *, *, #1428, .T. ) ;
#13101 = PRODUCT_DEFINITION_FORMATION_WITH_SPECIFIED_SOURCE ( 'ANY', '', #18865, .NOT_KNOWN. ) ;
#13102 = ADVANCED_FACE ( 'NONE', ( #21682 ), #13284, .F. ) ;
#13103 = DIRECTION ( 'NONE',  ( 0.000000000000000000, 0.000000000000000000, 1.000000000000000000 ) ) ;
#13104 = ORIENTED_EDGE ( 'NONE', *, *, #5464, .T. ) ;
#13105 = DIRECTION ( 'NONE',  ( 1.000000000000000000, 0.000000000000000000, 0.000000000000000000 ) ) ;
#13106 = CYLINDRICAL_SURFACE ( 'NONE', #17267, 100.0000000000000000 ) ;
#13107 = ORIENTED_EDGE ( 'NONE', *, *, #20321, .F. ) ;
#13108 = CARTESIAN_POINT ( 'NONE',  ( 10.00000000000000000, -19.83954325428602061, -82.71385593638713374 ) ) ;
#13110 = EDGE_CURVE ( 'NONE', #14138, #3479, #9737, .T. ) ;
#13109 = VERTEX_POINT ( 'NONE', #13066 ) ;
#13111 = EDGE_LOOP ( 'NONE', ( #16037, #13248, #13501, #6199 ) ) ;
#13112 = ADVANCED_FACE ( 'NONE', ( #6240 ), #13400, .F. ) ;
#13113 = CARTESIAN_POINT ( 'NONE',  ( -10.00000000000000888, 0.000000000000000000, -103.6250000000000284 ) ) ;
#13114 = ORIENTED_EDGE ( 'NONE', *, *, #17021, .F. ) ;
#13115 = DIRECTION ( 'NONE',  ( 1.000000000000000000, 0.000000000000000000, 0.000000000000000000 ) ) ;
#13116 = EDGE_CURVE ( 'NONE', #923, #14609, #7883, .T. ) ;
#13117 = DIRECTION ( 'NONE',  ( -0.8831157194574072999, 0.000000000000000000, 0.4691552259617553511 ) ) ;
#13118 = CARTESIAN_POINT ( 'NONE',  ( 10.00000000000000000, -28.00896854771981026, -15.47571261340951132 ) ) ;
#13119 = AXIS2_PLACEMENT_3D ( 'NONE', #12435, #309, #20626 ) ;
#13120 = DIRECTION ( 'NONE',  ( -1.000000000000000000, -0.000000000000000000, -0.000000000000000000 ) ) ;
#13121 = CARTESIAN_POINT ( 'NONE',  ( 0.000000000000000000, -2.481790431838652111, -92.46770094066596357 ) ) ;
#13122 = CARTESIAN_POINT ( 'NONE',  ( -1.399999999999998579, 0.000000000000000000, -7.500000000000020428 ) ) ;
#13123 = CYLINDRICAL_SURFACE ( 'NONE', #16905, 44.99999999999999289 ) ;
#13124 = EDGE_CURVE ( 'NONE', #378, #14927, #20349, .T. ) ;
#13125 = FACE_OUTER_BOUND ( 'NONE', #13547, .T. ) ;
#13126 = EDGE_CURVE ( 'NONE', #17521, #1324, #5867, .T. ) ;
#13127 = DIRECTION ( 'NONE',  ( 0.000000000000000000, 0.000000000000000000, -1.000000000000000000 ) ) ;
#13128 = EDGE_LOOP ( 'NONE', ( #4856, #9204, #14009, #5920 ) ) ;
#13129 = ORIENTED_EDGE ( 'NONE', *, *, #9150, .F. ) ;
#13130 = EDGE_CURVE ( 'NONE', #6690, #6258, #4571, .T. ) ;
#13131 = ORIENTED_EDGE ( 'NONE', *, *, #19445, .F. ) ;
#13132 = CIRCLE ( 'NONE', #2901, 27.49900000000000233 ) ;
#13133 = ORIENTED_EDGE ( 'NONE', *, *, #11770, .F. ) ;
#13134 = ORIENTED_EDGE ( 'NONE', *, *, #5564, .T. ) ;
#13135 = CARTESIAN_POINT ( 'NONE',  ( 10.00000000000000000, -60.65279801375299229, -63.75921967137679047 ) ) ;
#13136 = CIRCLE ( 'NONE', #3272, 45.00000000000000000 ) ;
#13137 = EDGE_CURVE ( 'NONE', #18255, #1046, #18222, .T. ) ;
#13138 = ORIENTED_EDGE ( 'NONE', *, *, #12799, .F. ) ;
#13139 = DIRECTION ( 'NONE',  ( 0.000000000000000000, 0.000000000000000000, 1.000000000000000000 ) ) ;
#13140 = LINE ( 'NONE', #15130, #7509 ) ;
#13141 = AXIS2_PLACEMENT_3D ( 'NONE', #10249, #8813, #15438 ) ;
#13142 = CARTESIAN_POINT ( 'NONE',  ( 0.000000000000000000, 68.93609746931163329, 54.69748134696484954 ) ) ;
#13143 = CARTESIAN_POINT ( 'NONE',  ( 10.00000000000000000, 0.000000000000000000, 0.000000000000000000 ) ) ;
#13144 = SURFACE_STYLE_FILL_AREA ( #4757 ) ;
#13145 = CARTESIAN_POINT ( 'NONE',  ( 10.00000000000000000, 75.27139873020959726, -53.76477968147737840 ) ) ;
#13146 = CARTESIAN_POINT ( 'NONE',  ( 10.00000000000000000, 15.51843147776463638, -83.63233659819634624 ) ) ;
#13147 = VECTOR ( 'NONE', #14811, 1000.000000000000000 ) ;
#13148 = VERTEX_POINT ( 'NONE', #9627 ) ;
#13149 = DIRECTION ( 'NONE',  ( 0.000000000000000000, -7.093091546216279124E-15, 1.000000000000000000 ) ) ;
#13150 = VECTOR ( 'NONE', #2418, 1000.000000000000000 ) ;
#13151 = AXIS2_PLACEMENT_3D ( 'NONE', #7172, #20547, #20646 ) ;
#13152 = ORIENTED_EDGE ( 'NONE', *, *, #13508, .F. ) ;
#13153 = AXIS2_PLACEMENT_3D ( 'NONE', #10418, #8766, #21350 ) ;
#13154 = EDGE_CURVE ( 'NONE', #6764, #5377, #19629, .T. ) ;
#13155 = EDGE_LOOP ( 'NONE', ( #14597, #2495, #13410, #7299 ) ) ;
#13156 = CARTESIAN_POINT ( 'NONE',  ( 0.000000000000000000, 13.56333590714014825, 28.98337314858439839 ) ) ;
#13157 = EDGE_LOOP ( 'NONE', ( #14068, #5331, #7991, #14095 ) ) ;
#13158 = CARTESIAN_POINT ( 'NONE',  ( 0.000000000000000000, 0.000000000000000000, 0.000000000000000000 ) ) ;
#13159 = VERTEX_POINT ( 'NONE', #9860 ) ;
#13160 = ORIENTED_EDGE ( 'NONE', *, *, #41, .T. ) ;
#13161 = FACE_OUTER_BOUND ( 'NONE', #13035, .T. ) ;
#13162 = AXIS2_PLACEMENT_3D ( 'NONE', #1425, #11351, #21629 ) ;
#13163 = ORIENTED_EDGE ( 'NONE', *, *, #21593, .F. ) ;
#13164 = CARTESIAN_POINT ( 'NONE',  ( 5.000000000000002665, 5.479102470011647519, -87.82926298292107958 ) ) ;
#13165 = CARTESIAN_POINT ( 'NONE',  ( 10.00000000000000000, 77.39385041987151226, -35.28996114464630551 ) ) ;
#13166 = CARTESIAN_POINT ( 'NONE',  ( 10.00000000000000000, 90.32141448704707898, -19.96189084378132961 ) ) ;
#13167 = CARTESIAN_POINT ( 'NONE',  ( 7.395799999999999486, 0.000000000000000000, 0.000000000000000000 ) ) ;
#13168 = SURFACE_STYLE_FILL_AREA ( #4671 ) ;
#13169 = DIRECTION ( 'NONE',  ( 0.000000000000000000, -0.9993908270190954291, -0.03489949670251119018 ) ) ;
#13170 = FACE_OUTER_BOUND ( 'NONE', #20579, .T. ) ;
#13171 = CARTESIAN_POINT ( 'NONE',  ( 0.000000000000000000, 0.000000000000000000, 0.000000000000000000 ) ) ;
#13172 = CARTESIAN_POINT ( 'NONE',  ( -2.000000000000000000, 70.00000000000000000, 9.999999999999998224 ) ) ;
#13173 = AXIS2_PLACEMENT_3D ( 'NONE', #2903, #6353, #3124 ) ;
#13174 = VERTEX_POINT ( 'NONE', #4898 ) ;
#13175 = AXIS2_PLACEMENT_3D ( 'NONE', #15546, #3513, #408 ) ;
#13176 = CARTESIAN_POINT ( 'NONE',  ( 7.999999999999979572, 0.000000000000000000, 0.000000000000000000 ) ) ;
#13177 = AXIS2_PLACEMENT_3D ( 'NONE', #4574, #21580, #7999 ) ;
#13178 = DIRECTION ( 'NONE',  ( -1.000000000000000000, -0.000000000000000000, 0.000000000000000000 ) ) ;
#13179 = ORIENTED_EDGE ( 'NONE', *, *, #1270, .F. ) ;
#13180 = CARTESIAN_POINT ( 'NONE',  ( 10.49999999999999822, 1.285879139104720633E-15, 3.000000000000000000 ) ) ;
#13181 = VERTEX_POINT ( 'NONE', #9961 ) ;
#13182 = CIRCLE ( 'NONE', #2608, 44.99999999999999289 ) ;
#13183 =( NAMED_UNIT ( * ) PLANE_ANGLE_UNIT ( ) SI_UNIT ( $, .RADIAN. ) );
#13184 = ORIENTED_EDGE ( 'NONE', *, *, #11633, .T. ) ;
#13185 = FACE_OUTER_BOUND ( 'NONE', #19723, .T. ) ;
#13186 = VERTEX_POINT ( 'NONE', #11409 ) ;
#13187 = VERTEX_POINT ( 'NONE', #19810 ) ;
#13188 = CARTESIAN_POINT ( 'NONE',  ( 10.00000000000000000, -12.46320060045702682, -29.47318494484041196 ) ) ;
#13189 = CARTESIAN_POINT ( 'NONE',  ( 5.000000000000002665, 87.58454185039451545, -8.540961822680756654 ) ) ;
#13190 = EDGE_LOOP ( 'NONE', ( #9555, #4805, #476, #8284 ) ) ;
#13191 = VECTOR ( 'NONE', #9990, 1000.000000000000000 ) ;
#13192 = CARTESIAN_POINT ( 'NONE',  ( 10.00000000000000000, 90.32141448704683739, 19.96189084378252332 ) ) ;
#13193 = LINE ( 'NONE', #12985, #6645 ) ;
#13194 = FACE_OUTER_BOUND ( 'NONE', #14301, .T. ) ;
#13195 = CARTESIAN_POINT ( 'NONE',  ( 0.000000000000000000, 81.97107881582195432, 22.71412948308594437 ) ) ;
#13196 = FACE_OUTER_BOUND ( 'NONE', #6373, .T. ) ;
#13197 = CARTESIAN_POINT ( 'NONE',  ( 5.000000000000000000, -19.29292659243987629, -25.53004080487782090 ) ) ;
#13198 = UNCERTAINTY_MEASURE_WITH_UNIT (LENGTH_MEASURE( 1.000000000000000082E-05 ), #14525, 'distance_accuracy_value', 'NONE');
#13199 = APPLICATION_CONTEXT ( 'automotive_design' ) ;
#13200 = VERTEX_POINT ( 'NONE', #3018 ) ;
#13201 = VECTOR ( 'NONE', #596, 1000.000000000000000 ) ;
#13202 = CYLINDRICAL_SURFACE ( 'NONE', #10226, 44.99999999999999289 ) ;
#13203 = DIRECTION ( 'NONE',  ( -1.000000000000000000, -0.000000000000000000, -0.000000000000000000 ) ) ;
#13204 = EDGE_CURVE ( 'NONE', #2153, #20998, #16497, .T. ) ;
#13205 = ORIENTED_EDGE ( 'NONE', *, *, #20228, .F. ) ;
#13206 = DIRECTION ( 'NONE',  ( 0.000000000000000000, 0.000000000000000000, 1.000000000000000000 ) ) ;
#13207 = ORIENTED_EDGE ( 'NONE', *, *, #11613, .F. ) ;
#13208 = AXIS2_PLACEMENT_3D ( 'NONE', #20656, #2103, #7179 ) ;
#13209 = DIRECTION ( 'NONE',  ( 0.000000000000000000, -0.9702957262759988044, 0.2419218955996583209 ) ) ;
#13210 = AXIS2_PLACEMENT_3D ( 'NONE', #7316, #11591, #11360 ) ;
#13211 = DIRECTION ( 'NONE',  ( -1.000000000000000000, -0.000000000000000000, 0.000000000000000000 ) ) ;
#13212 = EDGE_LOOP ( 'NONE', ( #5842, #13488 ) ) ;
#13213 = EDGE_CURVE ( 'NONE', #16808, #19662, #13263, .T. ) ;
#13214 = FACE_OUTER_BOUND ( 'NONE', #19969, .T. ) ;
#13215 = AXIS2_PLACEMENT_3D ( 'NONE', #17179, #15397, #10101 ) ;
#13216 = ORIENTED_EDGE ( 'NONE', *, *, #13525, .F. ) ;
#13217 = ORIENTED_EDGE ( 'NONE', *, *, #11228, .F. ) ;
#13218 = CARTESIAN_POINT ( 'NONE',  ( 10.00000000000000000, 0.000000000000000000, 0.000000000000000000 ) ) ;
#13219 = VECTOR ( 'NONE', #9568, 1000.000000000000000 ) ;
#13220 = ORIENTED_EDGE ( 'NONE', *, *, #15167, .F. ) ;
#13221 = EDGE_CURVE ( 'NONE', #5691, #12772, #11735, .T. ) ;
#13222 = DIRECTION ( 'NONE',  ( -1.000000000000000000, 0.000000000000000000, 0.000000000000000000 ) ) ;
#13223 = DIRECTION ( 'NONE',  ( 0.000000000000000000, -0.9702957262759988044, 0.2419218955996583209 ) ) ;
#13224 = CARTESIAN_POINT ( 'NONE',  ( -8.000000000000007105, 0.000000000000000000, 0.000000000000000000 ) ) ;
#13225 = DIRECTION ( 'NONE',  ( -1.000000000000000000, 0.000000000000000000, 0.000000000000000000 ) ) ;
#13226 = DIRECTION ( 'NONE',  ( 1.000000000000000000, 0.000000000000000000, 0.000000000000000000 ) ) ;
#13227 = CIRCLE ( 'NONE', #1942, 101.1000000000000369 ) ;
#13228 = CARTESIAN_POINT ( 'NONE',  ( 0.000000000000000000, 0.000000000000000000, 0.000000000000000000 ) ) ;
#13229 = VECTOR ( 'NONE', #14974, 1000.000000000000000 ) ;
#13230 = CARTESIAN_POINT ( 'NONE',  ( 123.5000000000000142, 0.000000000000000000, -3.000000000000000000 ) ) ;
#13231 = CIRCLE ( 'NONE', #10768, 88.00000000000000000 ) ;
#13232 = DIRECTION ( 'NONE',  ( -1.000000000000000000, -0.000000000000000000, 0.000000000000000000 ) ) ;
#13233 = AXIS2_PLACEMENT_3D ( 'NONE', #21470, #21250, #6352 ) ;
#13234 = EDGE_CURVE ( 'NONE', #17607, #4602, #12061, .T. ) ;
#13235 = CYLINDRICAL_SURFACE ( 'NONE', #184, 44.99999999999999289 ) ;
#13236 = EDGE_CURVE ( 'NONE', #2109, #2060, #17519, .T. ) ;
#13237 = EDGE_CURVE ( 'NONE', #7101, #19710, #9032, .T. ) ;
#13238 = VECTOR ( 'NONE', #1310, 1000.000000000000000 ) ;
#13239 = CARTESIAN_POINT ( 'NONE',  ( 0.000000000000000000, 0.000000000000000000, 0.000000000000000000 ) ) ;
#13240 = ORIENTED_EDGE ( 'NONE', *, *, #1678, .F. ) ;
#13241 = EDGE_CURVE ( 'NONE', #12017, #17526, #8856, .T. ) ;
#13242 = ORIENTED_EDGE ( 'NONE', *, *, #11380, .T. ) ;
#13243 = EDGE_LOOP ( 'NONE', ( #16543, #12614, #4509, #20968 ) ) ;
#13244 = EDGE_LOOP ( 'NONE', ( #15987, #14747 ) ) ;
#13245 = VECTOR ( 'NONE', #11085, 1000.000000000000000 ) ;
#13246 = VECTOR ( 'NONE', #4653, 1000.000000000000000 ) ;
#13247 = AXIS2_PLACEMENT_3D ( 'NONE', #6481, #20063, #4814 ) ;
#13248 = ORIENTED_EDGE ( 'NONE', *, *, #13687, .T. ) ;
#13249 = EDGE_CURVE ( 'NONE', #739, #16104, #15594, .T. ) ;
#13250 = CARTESIAN_POINT ( 'NONE',  ( 10.00000000000000000, 21.65267340503369198, -89.93106657554412209 ) ) ;
#13251 = ORIENTED_EDGE ( 'NONE', *, *, #4369, .T. ) ;
#13252 = CARTESIAN_POINT ( 'NONE',  ( 10.00000000000000000, 15.51843147776463638, -83.63233659819634624 ) ) ;
#13253 = CARTESIAN_POINT ( 'NONE',  ( 8.899999999999991473, 0.000000000000000000, -120.0000000000000568 ) ) ;
#13254 = ADVANCED_FACE ( 'NONE', ( #15161 ), #16824, .T. ) ;
#13255 = DIRECTION ( 'NONE',  ( 0.000000000000000000, 0.000000000000000000, 1.000000000000000000 ) ) ;
#13256 = DIRECTION ( 'NONE',  ( 0.000000000000000000, 0.000000000000000000, 1.000000000000000000 ) ) ;
#13257 = DIRECTION ( 'NONE',  ( 0.000000000000000000, 0.000000000000000000, -1.000000000000000000 ) ) ;
#13258 = DIRECTION ( 'NONE',  ( 0.000000000000000000, -6.982962677686266711E-15, 1.000000000000000000 ) ) ;
#13259 = CARTESIAN_POINT ( 'NONE',  ( 10.00000000000000000, 7.619321854369562885, 26.42235673590693423 ) ) ;
#13260 = CIRCLE ( 'NONE', #12914, 45.00000000000000711 ) ;
#13261 = EDGE_LOOP ( 'NONE', ( #18668, #18326, #11399, #12892 ) ) ;
#13262 = AXIS2_PLACEMENT_3D ( 'NONE', #19235, #4209, #14251 ) ;
#13263 = CIRCLE ( 'NONE', #576, 92.50100000000001899 ) ;
#13264 = CARTESIAN_POINT ( 'NONE',  ( 10.00000000000000000, -81.83745710415254848, -32.35167097270233683 ) ) ;
#13265 = VECTOR ( 'NONE', #5844, 1000.000000000000000 ) ;
#13266 = ADVANCED_FACE ( 'NONE', ( #16942 ), #1899, .F. ) ;
#13267 = ORIENTED_EDGE ( 'NONE', *, *, #12454, .T. ) ;
#13268 = ORIENTED_EDGE ( 'NONE', *, *, #14089, .T. ) ;
#13269 = CARTESIAN_POINT ( 'NONE',  ( 0.000000000000000000, 28.15804365424197186, -1.358152127006073684 ) ) ;
#13270 = ORIENTED_EDGE ( 'NONE', *, *, #7167, .T. ) ;
#13271 = DIRECTION ( 'NONE',  ( -1.000000000000000000, -0.000000000000000000, -0.000000000000000000 ) ) ;
#13272 = ORIENTED_EDGE ( 'NONE', *, *, #6903, .F. ) ;
#13273 = VERTEX_POINT ( 'NONE', #15261 ) ;
#13274 = EDGE_CURVE ( 'NONE', #18351, #13474, #11506, .T. ) ;
#13275 = DIRECTION ( 'NONE',  ( -1.000000000000000000, 0.000000000000000000, -0.000000000000000000 ) ) ;
#13276 = VERTEX_POINT ( 'NONE', #464 ) ;
#13277 = AXIS2_PLACEMENT_3D ( 'NONE', #11261, #20989, #4528 ) ;
#13278 = DIRECTION ( 'NONE',  ( 0.000000000000000000, 0.9848077530122073542, 0.1736481776669339949 ) ) ;
#13279 = EDGE_CURVE ( 'NONE', #14957, #16786, #18598, .T. ) ;
#13280 = VECTOR ( 'NONE', #4872, 1000.000000000000000 ) ;
#13281 = DIRECTION ( 'NONE',  ( -1.000000000000000000, 0.000000000000000000, -0.000000000000000000 ) ) ;
#13282 = LINE ( 'NONE', #13398, #6200 ) ;
#13283 = CARTESIAN_POINT ( 'NONE',  ( 0.000000000000000000, 31.75612719289746266, -3.943144139962234451 ) ) ;
#13284 = CYLINDRICAL_SURFACE ( 'NONE', #16805, 44.99999999999998579 ) ;
#13285 = EDGE_CURVE ( 'NONE', #18956, #13661, #7206, .T. ) ;
#13286 = EDGE_CURVE ( 'NONE', #19526, #3248, #1292, .T. ) ;
#13287 = DIRECTION ( 'NONE',  ( 0.000000000000000000, 1.000000000000000000, 0.000000000000000000 ) ) ;
#13288 = LINE ( 'NONE', #20036, #20680 ) ;
#13289 = FACE_OUTER_BOUND ( 'NONE', #5023, .T. ) ;
#13290 = ORIENTED_EDGE ( 'NONE', *, *, #6863, .F. ) ;
#13291 = VECTOR ( 'NONE', #4650, 1000.000000000000000 ) ;
#13292 = AXIS2_PLACEMENT_3D ( 'NONE', #5144, #271, #2037 ) ;
#13293 = CIRCLE ( 'NONE', #16103, 32.00000000000000000 ) ;
#13294 = VECTOR ( 'NONE', #2522, 1000.000000000000000 ) ;
#13295 = DIRECTION ( 'NONE',  ( 0.000000000000000000, -1.000000000000000000, 0.000000000000000000 ) ) ;
#13296 = CARTESIAN_POINT ( 'NONE',  ( 5.000000000000000888, -30.24235385705245349, 10.45944707835097454 ) ) ;
#13297 = VERTEX_POINT ( 'NONE', #3455 ) ;
#13298 = PLANE ( 'NONE',  #1045 ) ;
#13299 = ORIENTED_EDGE ( 'NONE', *, *, #16048, .F. ) ;
#13300 = ORIENTED_EDGE ( 'NONE', *, *, #248, .F. ) ;
#13301 = CARTESIAN_POINT ( 'NONE',  ( -1.500000000000000000, 15.00000000000000000, 0.000000000000000000 ) ) ;
#13302 = EDGE_LOOP ( 'NONE', ( #1564, #9880, #1279, #8095 ) ) ;
#13303 = ORIENTED_EDGE ( 'NONE', *, *, #1217, .T. ) ;
#13304 = DIRECTION ( 'NONE',  ( -1.000000000000000000, 0.000000000000000000, -0.000000000000000000 ) ) ;
#13305 = DIRECTION ( 'NONE',  ( -1.000000000000000000, 0.000000000000000000, 0.000000000000000000 ) ) ;
#13306 = VERTEX_POINT ( 'NONE', #8434 ) ;
#13307 = AXIS2_PLACEMENT_3D ( 'NONE', #3433, #1776, #14462 ) ;
#13308 = FACE_OUTER_BOUND ( 'NONE', #20415, .T. ) ;
#13309 = CARTESIAN_POINT ( 'NONE',  ( 0.000000000000000000, 0.000000000000000000, 0.000000000000000000 ) ) ;
#13310 = CIRCLE ( 'NONE', #6614, 11.99999999999999822 ) ;
#13311 = DIRECTION ( 'NONE',  ( -1.000000000000000000, -0.000000000000000000, -0.000000000000000000 ) ) ;
#13312 = CARTESIAN_POINT ( 'NONE',  ( 1.500000000000000888, 0.000000000000000000, -5.100000000000000533 ) ) ;
#13313 = CIRCLE ( 'NONE', #8743, 11.99999999999999645 ) ;
#13314 = LINE ( 'NONE', #18193, #12457 ) ;
#13315 = DIRECTION ( 'NONE',  ( 1.000000000000000000, 0.000000000000000000, 0.000000000000000000 ) ) ;
#13316 = ORIENTED_EDGE ( 'NONE', *, *, #15004, .T. ) ;
#13317 = DIRECTION ( 'NONE',  ( 0.000000000000000000, 0.000000000000000000, 1.000000000000000000 ) ) ;
#13318 = CARTESIAN_POINT ( 'NONE',  ( 10.00000000000000000, 0.000000000000000000, 0.000000000000000000 ) ) ;
#13319 = ORIENTED_EDGE ( 'NONE', *, *, #11236, .F. ) ;
#13320 = FACE_OUTER_BOUND ( 'NONE', #5841, .T. ) ;
#13321 = VERTEX_POINT ( 'NONE', #249 ) ;
#13322 = VECTOR ( 'NONE', #5651, 1000.000000000000000 ) ;
#13323 = SURFACE_SIDE_STYLE ('',( #17081 ) ) ;
#13324 = AXIS2_PLACEMENT_3D ( 'NONE', #7459, #17844, #12747 ) ;
#13325 = AXIS2_PLACEMENT_3D ( 'NONE', #9007, #3509, #624 ) ;
#13326 = CARTESIAN_POINT ( 'NONE',  ( 10.00000000000000000, 0.000000000000000000, 0.000000000000000000 ) ) ;
#13327 = VECTOR ( 'NONE', #18925, 1000.000000000000000 ) ;
#13328 = VERTEX_POINT ( 'NONE', #18714 ) ;
#13329 =( NAMED_UNIT ( * ) SI_UNIT ( $, .STERADIAN. ) SOLID_ANGLE_UNIT ( ) );
#13330 = VERTEX_POINT ( 'NONE', #7105 ) ;
#13331 = VERTEX_POINT ( 'NONE', #6994 ) ;
#13332 = DIRECTION ( 'NONE',  ( 1.000000000000000000, 0.000000000000000000, 0.000000000000000000 ) ) ;
#13333 = ORIENTED_EDGE ( 'NONE', *, *, #13915, .T. ) ;
#13334 = APPLICATION_CONTEXT ( 'automotive_design' ) ;
#13335 = PLANE ( 'NONE',  #16918 ) ;
#13336 = DIRECTION ( 'NONE',  ( -1.000000000000000000, 0.000000000000000000, 0.000000000000000000 ) ) ;
#13337 = CARTESIAN_POINT ( 'NONE',  ( 10.00000000000000000, -3.974475837764312569, -92.41557521768193340 ) ) ;
#13338 = EDGE_CURVE ( 'NONE', #5362, #8003, #16455, .T. ) ;
#13339 = DIRECTION ( 'NONE',  ( 1.000000000000000000, 0.000000000000000000, -0.000000000000000000 ) ) ;
#13340 = VECTOR ( 'NONE', #7547, 1000.000000000000000 ) ;
#13341 = DIRECTION ( 'NONE',  ( 0.000000000000000000, 0.9945218953682729568, 0.1045284632676570791 ) ) ;
#13342 = DIRECTION ( 'NONE',  ( -0.000000000000000000, -0.000000000000000000, -1.000000000000000000 ) ) ;
#13343 = CIRCLE ( 'NONE', #11949, 44.99999999999999289 ) ;
#13344 = CIRCLE ( 'NONE', #21818, 44.99999999999999289 ) ;
#13345 = EDGE_CURVE ( 'NONE', #610, #13331, #244, .T. ) ;
#13346 = DIRECTION ( 'NONE',  ( 1.000000000000000000, 0.000000000000000000, -0.000000000000000000 ) ) ;
#13347 = CARTESIAN_POINT ( 'NONE',  ( 10.00000000000000000, -19.85071254963791176, 20.01672328094525000 ) ) ;
#13348 = CARTESIAN_POINT ( 'NONE',  ( 0.000000000000000000, 0.000000000000000000, 0.000000000000000000 ) ) ;
#13349 = ORIENTED_EDGE ( 'NONE', *, *, #5031, .F. ) ;
#13350 = DIRECTION ( 'NONE',  ( -1.000000000000000000, 0.000000000000000000, 0.000000000000000000 ) ) ;
#13351 = ORIENTED_EDGE ( 'NONE', *, *, #14980, .F. ) ;
#13352 = ORIENTED_EDGE ( 'NONE', *, *, #15912, .T. ) ;
#13353 = AXIS2_PLACEMENT_3D ( 'NONE', #1188, #9794, #2953 ) ;
#13354 = VERTEX_POINT ( 'NONE', #6886 ) ;
#13355 = AXIS2_PLACEMENT_3D ( 'NONE', #15118, #16899, #21338 ) ;
#13356 = CIRCLE ( 'NONE', #6684, 44.99999999999998579 ) ;
#13357 = AXIS2_PLACEMENT_3D ( 'NONE', #21099, #14352, #21206 ) ;
#13358 = EDGE_LOOP ( 'NONE', ( #7556, #19618 ) ) ;
#13359 = CARTESIAN_POINT ( 'NONE',  ( 0.000000000000000000, 0.000000000000000000, 0.000000000000000000 ) ) ;
#13360 = ORIENTED_EDGE ( 'NONE', *, *, #13801, .T. ) ;
#13361 = DIRECTION ( 'NONE',  ( 0.000000000000000000, 0.7880107536067231244, -0.6156614753256566264 ) ) ;
#13362 = ADVANCED_FACE ( 'NONE', ( #5225 ), #18808, .F. ) ;
#13363 = EDGE_CURVE ( 'NONE', #3486, #14906, #17154, .T. ) ;
#13364 = ADVANCED_FACE ( 'NONE', ( #5547 ), #9272, .F. ) ;
#13365 = DIRECTION ( 'NONE',  ( -1.000000000000000000, -0.000000000000000000, -0.000000000000000000 ) ) ;
#13366 = EDGE_CURVE ( 'NONE', #6258, #4702, #20362, .T. ) ;
#13367 = CARTESIAN_POINT ( 'NONE',  ( -10.00000000000000000, 0.000000000000000000, 0.000000000000000000 ) ) ;
#13368 = DIRECTION ( 'NONE',  ( -1.000000000000000000, -0.000000000000000000, -0.000000000000000000 ) ) ;
#13369 = CARTESIAN_POINT ( 'NONE',  ( 10.00000000000000000, -35.18804927320473297, -80.65854690202716881 ) ) ;
#13370 = DIRECTION ( 'NONE',  ( -1.000000000000000000, 0.000000000000000000, -0.000000000000000000 ) ) ;
#13371 = VECTOR ( 'NONE', #3397, 1000.000000000000000 ) ;
#13372 = CIRCLE ( 'NONE', #15488, 88.00000000000000000 ) ;
#13373 = CIRCLE ( 'NONE', #5264, 5.000000000000000000 ) ;
#13374 = ORIENTED_EDGE ( 'NONE', *, *, #18368, .T. ) ;
#13376 = CIRCLE ( 'NONE', #18350, 92.50099999999999056 ) ;
#13375 = PRODUCT_DEFINITION_SHAPE ( 'NONE', 'NONE',  #21865 ) ;
#13377 = DIRECTION ( 'NONE',  ( -1.000000000000000000, 0.000000000000000000, 0.000000000000000000 ) ) ;
#13378 = ADVANCED_FACE ( 'NONE', ( #2541 ), #2448, .F. ) ;
#13379 = EDGE_LOOP ( 'NONE', ( #13717, #19170, #16268, #189 ) ) ;
#13380 = ORIENTED_EDGE ( 'NONE', *, *, #18128, .F. ) ;
#13381 = EDGE_CURVE ( 'NONE', #13692, #18297, #14699, .T. ) ;
#13382 = DIRECTION ( 'NONE',  ( 0.000000000000000000, -0.8660254037844432595, 0.4999999999999920064 ) ) ;
#13383 = VERTEX_POINT ( 'NONE', #7638 ) ;
#13384 = DIRECTION ( 'NONE',  ( -1.000000000000000000, -0.000000000000000000, -0.000000000000000000 ) ) ;
#13385 = VERTEX_POINT ( 'NONE', #21007 ) ;
#13386 = EDGE_LOOP ( 'NONE', ( #9489, #21529 ) ) ;
#13387 = SHAPE_DEFINITION_REPRESENTATION ( #15319, #14169 ) ;
#13388 = AXIS2_PLACEMENT_3D ( 'NONE', #1571, #18271, #13396 ) ;
#13389 = CARTESIAN_POINT ( 'NONE',  ( -10.00000000000000000, 0.000000000000000000, 0.000000000000000000 ) ) ;
#13390 = ORIENTED_EDGE ( 'NONE', *, *, #145, .T. ) ;
#13391 = AXIS2_PLACEMENT_3D ( 'NONE', #5593, #294, #10557 ) ;
#13392 = EDGE_CURVE ( 'NONE', #4414, #4038, #17887, .T. ) ;
#13393 = DIRECTION ( 'NONE',  ( -1.000000000000000000, 0.000000000000000000, -0.000000000000000000 ) ) ;
#13394 = AXIS2_PLACEMENT_3D ( 'NONE', #3597, #19964, #4828 ) ;
#13395 = AXIS2_PLACEMENT_3D ( 'NONE', #8379, #2081, #13789 ) ;
#13396 = DIRECTION ( 'NONE',  ( 0.000000000000000000, 0.000000000000000000, 1.000000000000000000 ) ) ;
#13397 = ADVANCED_FACE ( 'NONE', ( #20793 ), #10817, .T. ) ;
#13398 = CARTESIAN_POINT ( 'NONE',  ( 5.000000000000002665, -40.72878876293203376, 78.00747250042435610 ) ) ;
#13399 = DIRECTION ( 'NONE',  ( -1.000000000000000000, 0.000000000000000000, 0.000000000000000000 ) ) ;
#13400 = CYLINDRICAL_SURFACE ( 'NONE', #10090, 44.99999999999999289 ) ;
#13401 = DIRECTION ( 'NONE',  ( 0.000000000000000000, -8.943463253924872306E-15, -1.000000000000000000 ) ) ;
#13402 = CARTESIAN_POINT ( 'NONE',  ( 0.000000000000000000, 0.000000000000000000, -3.000000000000000000 ) ) ;
#13403 = DIRECTION ( 'NONE',  ( -1.000000000000000000, -0.000000000000000000, -0.000000000000000000 ) ) ;
#13404 = ORIENTED_EDGE ( 'NONE', *, *, #11060, .T. ) ;
#13405 = EDGE_CURVE ( 'NONE', #667, #10646, #8702, .T. ) ;
#13406 = COLOUR_RGB ( '', 0.31764706, 0.68627451, 0.89019608) ;
#13407 = EDGE_CURVE ( 'NONE', #19953, #589, #5881, .T. ) ;
#13408 = DIRECTION ( 'NONE',  ( 0.000000000000000000, 0.000000000000000000, -1.000000000000000000 ) ) ;
#13409 = DIRECTION ( 'NONE',  ( 0.000000000000000000, 0.000000000000000000, 1.000000000000000000 ) ) ;
#13410 = ORIENTED_EDGE ( 'NONE', *, *, #831, .F. ) ;
#13411 = EDGE_CURVE ( 'NONE', #4965, #16375, #3888, .T. ) ;
#13412 = DIRECTION ( 'NONE',  ( 0.000000000000000000, 0.000000000000000000, -1.000000000000000000 ) ) ;
#13413 = ORIENTED_EDGE ( 'NONE', *, *, #16458, .T. ) ;
#13414 = EDGE_CURVE ( 'NONE', #15191, #21786, #10620, .T. ) ;
#13415 = VERTEX_POINT ( 'NONE', #12384 ) ;
#13416 = DIRECTION ( 'NONE',  ( 0.000000000000000000, 0.000000000000000000, -1.000000000000000000 ) ) ;
#13417 = EDGE_LOOP ( 'NONE', ( #20105, #19996, #12108, #9791 ) ) ;
#13418 = ORIENTED_EDGE ( 'NONE', *, *, #10802, .F. ) ;
#13419 = CARTESIAN_POINT ( 'NONE',  ( 0.000000000000000000, 62.44821182181184582, -68.23969402963440700 ) ) ;
#13420 = DIRECTION ( 'NONE',  ( 1.000000000000000000, 0.000000000000000000, 0.000000000000000000 ) ) ;
#13421 = EDGE_LOOP ( 'NONE', ( #16695, #18475, #7308, #121 ) ) ;
#13422 = EDGE_CURVE ( 'NONE', #10755, #20618, #2696, .T. ) ;
#13423 = CARTESIAN_POINT ( 'NONE',  ( -1.200000000000006617, 0.000000000000000000, 0.000000000000000000 ) ) ;
#13424 = CARTESIAN_POINT ( 'NONE',  ( 0.000000000000000000, 0.000000000000000000, 0.000000000000000000 ) ) ;
#13425 = DIRECTION ( 'NONE',  ( 0.000000000000000000, 1.000000000000000000, -1.224646799147353207E-16 ) ) ;
#13426 = DIRECTION ( 'NONE',  ( -1.000000000000000000, -0.000000000000000000, 0.000000000000000000 ) ) ;
#13427 = FACE_OUTER_BOUND ( 'NONE', #19146, .T. ) ;
#13428 = DIRECTION ( 'NONE',  ( 1.000000000000000000, 0.000000000000000000, 0.000000000000000000 ) ) ;
#13429 = EDGE_LOOP ( 'NONE', ( #8093, #21385, #8803, #8415 ) ) ;
#13430 = CARTESIAN_POINT ( 'NONE',  ( 10.00000000000000000, 27.48365448817206769, -0.9185515634842869037 ) ) ;
#13431 = CARTESIAN_POINT ( 'NONE',  ( 1.200000000000006617, 0.000000000000000000, 0.000000000000000000 ) ) ;
#13432 = ORIENTED_EDGE ( 'NONE', *, *, #20532, .T. ) ;
#13433 = DIRECTION ( 'NONE',  ( -1.000000000000000000, 0.000000000000000000, -0.000000000000000000 ) ) ;
#13434 = ORIENTED_EDGE ( 'NONE', *, *, #19216, .F. ) ;
#13435 = DIRECTION ( 'NONE',  ( 1.000000000000000000, 0.000000000000000000, 0.000000000000000000 ) ) ;
#13436 = VECTOR ( 'NONE', #2115, 1000.000000000000000 ) ;
#13437 = DIRECTION ( 'NONE',  ( 0.000000000000000000, -0.06975647374413236623, 0.9975640502598237536 ) ) ;
#13438 = ORIENTED_EDGE ( 'NONE', *, *, #12062, .F. ) ;
#13439 = EDGE_CURVE ( 'NONE', #4886, #8622, #19240, .T. ) ;
#13440 = VERTEX_POINT ( 'NONE', #15920 ) ;
#13441 = VERTEX_POINT ( 'NONE', #2334 ) ;
#13442 = ORIENTED_EDGE ( 'NONE', *, *, #6819, .F. ) ;
#13443 = CARTESIAN_POINT ( 'NONE',  ( 0.000000000000000000, 0.000000000000000000, 0.000000000000000000 ) ) ;
#13444 = ORIENTED_EDGE ( 'NONE', *, *, #4405, .T. ) ;
#13445 = CARTESIAN_POINT ( 'NONE',  ( -10.00000000000000000, 0.000000000000000000, 0.000000000000000000 ) ) ;
#13446 = DIRECTION ( 'NONE',  ( 0.000000000000000000, -7.093091546216279124E-15, 1.000000000000000000 ) ) ;
#13447 = DIRECTION ( 'NONE',  ( 1.000000000000000000, 0.000000000000000000, 0.000000000000000000 ) ) ;
#13448 = DIRECTION ( 'NONE',  ( -0.000000000000000000, 0.000000000000000000, -1.000000000000000000 ) ) ;
#13449 = CYLINDRICAL_SURFACE ( 'NONE', #13162, 92.50100000000000477 ) ;
#13450 = LINE ( 'NONE', #17100, #9077 ) ;
#13451 = DIRECTION ( 'NONE',  ( 0.000000000000000000, 0.000000000000000000, -1.000000000000000000 ) ) ;
#13452 = DIRECTION ( 'NONE',  ( 0.000000000000000000, 0.3420201433256694901, -0.9396926207859080948 ) ) ;
#13453 = DIRECTION ( 'NONE',  ( -1.000000000000000000, -0.000000000000000000, -0.000000000000000000 ) ) ;
#13454 = CYLINDRICAL_SURFACE ( 'NONE', #11536, 92.50100000000000477 ) ;
#13455 = ORIENTED_EDGE ( 'NONE', *, *, #17872, .F. ) ;
#13456 = CYLINDRICAL_SURFACE ( 'NONE', #10879, 44.99999999999999289 ) ;
#13457 = EDGE_CURVE ( 'NONE', #3544, #4447, #777, .T. ) ;
#13458 = ORIENTED_EDGE ( 'NONE', *, *, #12312, .T. ) ;
#13459 = CYLINDRICAL_SURFACE ( 'NONE', #13355, 44.99999999999999289 ) ;
#13460 = EDGE_LOOP ( 'NONE', ( #10674, #20019, #3842, #18213 ) ) ;
#13461 = ORIENTED_EDGE ( 'NONE', *, *, #20788, .T. ) ;
#13462 = EDGE_CURVE ( 'NONE', #9164, #15549, #19296, .T. ) ;
#13463 = ORIENTED_EDGE ( 'NONE', *, *, #3013, .T. ) ;
#13464 = CARTESIAN_POINT ( 'NONE',  ( 10.00000000000000000, 57.47876254627143311, 62.70072803846409215 ) ) ;
#13465 = VERTEX_POINT ( 'NONE', #4215 ) ;
#13466 = CARTESIAN_POINT ( 'NONE',  ( 0.000000000000000000, -27.87320266523617107, 88.20158487341750231 ) ) ;
#13467 = CARTESIAN_POINT ( 'NONE',  ( 0.000000000000000000, 19.07277123396568896, -19.80970465344728737 ) ) ;
#13468 = VECTOR ( 'NONE', #11464, 1000.000000000000000 ) ;
#13469 = DIRECTION ( 'NONE',  ( -1.000000000000000000, -0.000000000000000000, -0.000000000000000000 ) ) ;
#13470 = FACE_OUTER_BOUND ( 'NONE', #2787, .T. ) ;
#13471 = DIRECTION ( 'NONE',  ( -1.000000000000000000, 0.000000000000000000, 0.000000000000000000 ) ) ;
#13472 = DIRECTION ( 'NONE',  ( 0.000000000000000000, 0.000000000000000000, 1.000000000000000000 ) ) ;
#13473 = CARTESIAN_POINT ( 'NONE',  ( 10.00000000000000000, -92.32475887865429343, 5.707354816230212791 ) ) ;
#13474 = VERTEX_POINT ( 'NONE', #19452 ) ;
#13475 = DIRECTION ( 'NONE',  ( 0.000000000000000000, 0.000000000000000000, 1.000000000000000000 ) ) ;
#13476 = AXIS2_PLACEMENT_3D ( 'NONE', #17262, #20569, #3773 ) ;
#13477 = EDGE_CURVE ( 'NONE', #13893, #18255, #927, .T. ) ;
#13478 = VERTEX_POINT ( 'NONE', #7426 ) ;
#13479 = ORIENTED_EDGE ( 'NONE', *, *, #6354, .F. ) ;
#13480 = DIRECTION ( 'NONE',  ( -1.000000000000000000, 0.000000000000000000, 0.000000000000000000 ) ) ;
#13481 = CIRCLE ( 'NONE', #14193, 0.2042000000000016025 ) ;
#13482 = EDGE_LOOP ( 'NONE', ( #21775, #17256, #6145, #13598 ) ) ;
#13483 = CARTESIAN_POINT ( 'NONE',  ( -10.49999999999999822, 0.000000000000000000, 0.000000000000000000 ) ) ;
#13484 = ORIENTED_EDGE ( 'NONE', *, *, #11496, .F. ) ;
#13485 = ORIENTED_EDGE ( 'NONE', *, *, #5833, .F. ) ;
#13486 = CIRCLE ( 'NONE', #455, 5.000000000000000000 ) ;
#13487 = CARTESIAN_POINT ( 'NONE',  ( 10.00000000000000000, -39.87723064937176076, 83.46401306393555330 ) ) ;
#13488 = ORIENTED_EDGE ( 'NONE', *, *, #1638, .F. ) ;
#13489 = CARTESIAN_POINT ( 'NONE',  ( 0.000000000000000000, -5.479102470009884485, -87.82926298292120748 ) ) ;
#13490 = ADVANCED_FACE ( 'NONE', ( #12487 ), #10836, .T. ) ;
#13491 = CIRCLE ( 'NONE', #15258, 27.49900000000000233 ) ;
#13492 = DIRECTION ( 'NONE',  ( 0.000000000000000000, -0.9510565162951503115, -0.3090169943749573322 ) ) ;
#13493 = CARTESIAN_POINT ( 'NONE',  ( 0.000000000000000000, 0.000000000000000000, 0.000000000000000000 ) ) ;
#13494 = CARTESIAN_POINT ( 'NONE',  ( 0.000000000000000000, 0.000000000000000000, 0.000000000000000000 ) ) ;
#13495 = DIRECTION ( 'NONE',  ( -1.000000000000000000, -0.000000000000000000, 0.000000000000000000 ) ) ;
#13496 = EDGE_CURVE ( 'NONE', #14549, #4382, #8295, .T. ) ;
#13497 = DIRECTION ( 'NONE',  ( 0.000000000000000000, 0.000000000000000000, 1.000000000000000000 ) ) ;
#13498 = DIRECTION ( 'NONE',  ( 1.000000000000000000, 0.000000000000000000, 0.000000000000000000 ) ) ;
#13499 = AXIS2_PLACEMENT_3D ( 'NONE', #18686, #9827, #3315 ) ;
#13500 = AXIS2_PLACEMENT_3D ( 'NONE', #12361, #5310, #17450 ) ;
#13501 = ORIENTED_EDGE ( 'NONE', *, *, #11752, .F. ) ;
#13502 = CIRCLE ( 'NONE', #4693, 92.50100000000000477 ) ;
#13503 = EDGE_CURVE ( 'NONE', #17231, #12265, #18030, .T. ) ;
#13504 = VECTOR ( 'NONE', #21223, 1000.000000000000000 ) ;
#13505 = ADVANCED_FACE ( 'NONE', ( #13042 ), #7849, .F. ) ;
#13506 = ADVANCED_FACE ( 'NONE', ( #9500 ), #2985, .F. ) ;
#13507 = DIRECTION ( 'NONE',  ( 0.000000000000000000, -0.9993908270190959842, 0.03489949670249112984 ) ) ;
#13508 = EDGE_CURVE ( 'NONE', #19853, #5771, #12810, .T. ) ;
#13509 = DIRECTION ( 'NONE',  ( 1.000000000000000000, 0.000000000000000000, 0.000000000000000000 ) ) ;
#13510 = VECTOR ( 'NONE', #18544, 1000.000000000000000 ) ;
#13511 = ORIENTED_EDGE ( 'NONE', *, *, #12177, .T. ) ;
#13512 = DIRECTION ( 'NONE',  ( -1.000000000000000000, -0.000000000000000000, -0.000000000000000000 ) ) ;
#13513 = VERTEX_POINT ( 'NONE', #1111 ) ;
#13514 =( NAMED_UNIT ( * ) PLANE_ANGLE_UNIT ( ) SI_UNIT ( $, .RADIAN. ) );
#13515 = ORIENTED_EDGE ( 'NONE', *, *, #3537, .T. ) ;
#13516 = AXIS2_PLACEMENT_3D ( 'NONE', #492, #2360, #19268 ) ;
#13518 = EDGE_CURVE ( 'NONE', #17357, #4335, #13647, .T. ) ;
#13517 = DIRECTION ( 'NONE',  ( 0.000000000000000000, 0.000000000000000000, 1.000000000000000000 ) ) ;
#13519 = ORIENTED_EDGE ( 'NONE', *, *, #3004, .F. ) ;
#13520 = ORIENTED_EDGE ( 'NONE', *, *, #6197, .T. ) ;
#13521 = DIRECTION ( 'NONE',  ( 0.000000000000000000, 0.000000000000000000, -1.000000000000000000 ) ) ;
#13522 = FACE_OUTER_BOUND ( 'NONE', #4636, .T. ) ;
#13523 = AXIS2_PLACEMENT_3D ( 'NONE', #20305, #1842, #5170 ) ;
#13524 = ORIENTED_EDGE ( 'NONE', *, *, #15981, .F. ) ;
#13525 = EDGE_CURVE ( 'NONE', #11814, #12538, #18234, .T. ) ;
#13526 = CIRCLE ( 'NONE', #7693, 88.00000000000000000 ) ;
#13527 = CARTESIAN_POINT ( 'NONE',  ( -90.00000000000000000, 0.000000000000000000, 0.000000000000000000 ) ) ;
#13528 = DIRECTION ( 'NONE',  ( 0.000000000000000000, 0.000000000000000000, 1.000000000000000000 ) ) ;
#13529 = CARTESIAN_POINT ( 'NONE',  ( 0.000000000000000000, 0.000000000000000000, 0.000000000000000000 ) ) ;
#13530 = CYLINDRICAL_SURFACE ( 'NONE', #17086, 44.99999999999999289 ) ;
#13531 = DIRECTION ( 'NONE',  ( 1.000000000000000000, 0.000000000000000000, -0.000000000000000000 ) ) ;
#13532 = EDGE_CURVE ( 'NONE', #715, #19694, #11522, .T. ) ;
#13533 = CARTESIAN_POINT ( 'NONE',  ( 10.00000000000000000, -12.94633825542249994, -24.26081875733348170 ) ) ;
#13534 = CIRCLE ( 'NONE', #14601, 44.99999999999999289 ) ;
#13535 = ORIENTED_EDGE ( 'NONE', *, *, #4203, .F. ) ;
#13536 = ADVANCED_FACE ( 'NONE', ( #21224, #4429 ), #9597, .T. ) ;
#13537 = DIRECTION ( 'NONE',  ( -1.000000000000000000, -0.000000000000000000, -0.000000000000000000 ) ) ;
#13538 = VECTOR ( 'NONE', #15493, 1000.000000000000000 ) ;
#13539 = DIRECTION ( 'NONE',  ( 0.000000000000000000, 0.8660254037844361541, 0.5000000000000041078 ) ) ;
#13540 = VERTEX_POINT ( 'NONE', #19787 ) ;
#13541 = CIRCLE ( 'NONE', #9630, 92.50100000000000477 ) ;
#13542 = DIRECTION ( 'NONE',  ( 0.000000000000000000, 0.000000000000000000, 1.000000000000000000 ) ) ;
#13543 = VERTEX_POINT ( 'NONE', #9713 ) ;
#13544 = EDGE_CURVE ( 'NONE', #18504, #13297, #14340, .T. ) ;
#13545 = CYLINDRICAL_SURFACE ( 'NONE', #8449, 11.99999999999999645 ) ;
#13546 = CYLINDRICAL_SURFACE ( 'NONE', #6696, 44.99999999999999289 ) ;
#13547 = EDGE_LOOP ( 'NONE', ( #4423, #3972, #12074, #1102 ) ) ;
#13548 = LINE ( 'NONE', #18532, #21214 ) ;
#13549 = AXIS2_PLACEMENT_3D ( 'NONE', #11766, #20170, #1397 ) ;
#13550 = ORIENTED_EDGE ( 'NONE', *, *, #9178, .T. ) ;
#13551 = ORIENTED_EDGE ( 'NONE', *, *, #9884, .T. ) ;
#13552 = ORIENTED_EDGE ( 'NONE', *, *, #3376, .F. ) ;
#13553 = CYLINDRICAL_SURFACE ( 'NONE', #13523, 32.00000000000000000 ) ;
#13554 = ORIENTED_EDGE ( 'NONE', *, *, #19605, .T. ) ;
#13555 = CARTESIAN_POINT ( 'NONE',  ( 10.00000000000000888, 3.673940397442060361E-16, -3.000000000000000444 ) ) ;
#13556 = VECTOR ( 'NONE', #20620, 1000.000000000000000 ) ;
#13557 = CARTESIAN_POINT ( 'NONE',  ( 0.000000000000000000, -87.17509410653603652, -30.93441398372672069 ) ) ;
#13558 = LINE ( 'NONE', #21736, #13468 ) ;
#13559 = DIRECTION ( 'NONE',  ( 0.000000000000000000, -0.8290375725550467312, 0.5591929034707392443 ) ) ;
#13560 = EDGE_CURVE ( 'NONE', #6732, #9001, #11168, .T. ) ;
#13561 = DIRECTION ( 'NONE',  ( 0.000000000000000000, 0.000000000000000000, -1.000000000000000000 ) ) ;
#13562 = CARTESIAN_POINT ( 'NONE',  ( 0.000000000000000000, 83.03980459022480431, -18.42770452393272862 ) ) ;
#13563 = EDGE_CURVE ( 'NONE', #18649, #19720, #3758, .T. ) ;
#13564 = EDGE_CURVE ( 'NONE', #1056, #14528, #16106, .T. ) ;
#13565 = DIRECTION ( 'NONE',  ( 0.000000000000000000, 0.000000000000000000, 1.000000000000000000 ) ) ;
#13566 = CIRCLE ( 'NONE', #6181, 123.0000000000000000 ) ;
#13567 = CARTESIAN_POINT ( 'NONE',  ( 10.00000000000000888, 2.828427124746190291, -1.000000000000000000 ) ) ;
#13568 = FACE_OUTER_BOUND ( 'NONE', #14322, .T. ) ;
#13569 = AXIS2_PLACEMENT_3D ( 'NONE', #13527, #8667, #11663 ) ;
#13570 = ORIENTED_EDGE ( 'NONE', *, *, #10695, .T. ) ;
#13571 = SURFACE_STYLE_USAGE ( .BOTH. , #8391 ) ;
#13572 = ORIENTED_EDGE ( 'NONE', *, *, #21793, .F. ) ;
#13573 = FACE_OUTER_BOUND ( 'NONE', #10263, .T. ) ;
#13574 = AXIS2_PLACEMENT_3D ( 'NONE', #11758, #1920, #8661 ) ;
#13575 = ORIENTED_EDGE ( 'NONE', *, *, #13392, .F. ) ;
#13576 = ORIENTED_EDGE ( 'NONE', *, *, #6548, .F. ) ;
#13577 = VERTEX_POINT ( 'NONE', #16352 ) ;
#13578 = DIRECTION ( 'NONE',  ( 0.000000000000000000, 0.000000000000000000, 1.000000000000000000 ) ) ;
#13579 = ORIENTED_EDGE ( 'NONE', *, *, #7, .T. ) ;
#13580 = CARTESIAN_POINT ( 'NONE',  ( 10.00000000000000000, -84.12297548659712731, 32.40974838672912028 ) ) ;
#13581 = CIRCLE ( 'NONE', #7231, 32.00000000000000000 ) ;
#13582 = DIRECTION ( 'NONE',  ( 1.000000000000000000, 0.000000000000000000, -0.000000000000000000 ) ) ;
#13583 = VECTOR ( 'NONE', #2851, 1000.000000000000000 ) ;
#13584 = AXIS2_PLACEMENT_3D ( 'NONE', #12276, #17366, #19126 ) ;
#13585 = CARTESIAN_POINT ( 'NONE',  ( 5.000000000000000000, -36.39558101400191958, 80.12091913260368869 ) ) ;
#13586 = DIRECTION ( 'NONE',  ( 0.000000000000000000, 0.000000000000000000, 1.000000000000000000 ) ) ;
#13587 = CYLINDRICAL_SURFACE ( 'NONE', #2630, 44.99999999999999289 ) ;
#13588 = AXIS2_PLACEMENT_3D ( 'NONE', #19316, #21087, #9468 ) ;
#13589 = DIRECTION ( 'NONE',  ( -1.000000000000000000, -0.000000000000000000, -0.000000000000000000 ) ) ;
#13590 = FACE_OUTER_BOUND ( 'NONE', #718, .T. ) ;
#13591 = VERTEX_POINT ( 'NONE', #20010 ) ;
#13592 = DIRECTION ( 'NONE',  ( 1.000000000000000000, 0.000000000000000000, 0.000000000000000000 ) ) ;
#13593 = CIRCLE ( 'NONE', #10056, 92.50100000000000477 ) ;
#13594 = CIRCLE ( 'NONE', #7591, 118.9000000000000199 ) ;
#13595 = VERTEX_POINT ( 'NONE', #8078 ) ;
#13596 = AXIS2_PLACEMENT_3D ( 'NONE', #6110, #790, #7652 ) ;
#13597 = MANIFOLD_SOLID_BREP ( 'Fillet1', #20659 ) ;
#13598 = ORIENTED_EDGE ( 'NONE', *, *, #10712, .T. ) ;
#13599 = AXIS2_PLACEMENT_3D ( 'NONE', #2774, #7750, #11377 ) ;
#13600 = CARTESIAN_POINT ( 'NONE',  ( 0.000000000000000000, 56.05743251323859511, 67.83483072893820065 ) ) ;
#13601 = VERTEX_POINT ( 'NONE', #3638 ) ;
#13602 = DIRECTION ( 'NONE',  ( 0.000000000000000000, 0.7880107536067231244, -0.6156614753256568484 ) ) ;
#13603 = VERTEX_POINT ( 'NONE', #6975 ) ;
#13604 = ORIENTED_EDGE ( 'NONE', *, *, #11063, .F. ) ;
#13605 = DIRECTION ( 'NONE',  ( 1.000000000000000000, 0.000000000000000000, 0.000000000000000000 ) ) ;
#13606 = ORIENTED_EDGE ( 'NONE', *, *, #13682, .T. ) ;
#13607 = DIRECTION ( 'NONE',  ( -1.000000000000000000, 0.000000000000000000, 0.000000000000000000 ) ) ;
#13608 = LINE ( 'NONE', #20364, #17836 ) ;
#13609 = FACE_OUTER_BOUND ( 'NONE', #8256, .T. ) ;
#13610 = ADVANCED_FACE ( 'NONE', ( #14814 ), #13703, .T. ) ;
#13611 = AXIS2_PLACEMENT_3D ( 'NONE', #1726, #177, #6927 ) ;
#13612 = CARTESIAN_POINT ( 'NONE',  ( 10.00000000000000000, -64.66851233300764079, 55.25552418572942059 ) ) ;
#13613 = AXIS2_PLACEMENT_3D ( 'NONE', #19485, #4351, #11089 ) ;
#13614 = CIRCLE ( 'NONE', #9364, 115.1000000000000227 ) ;
#13615 = CARTESIAN_POINT ( 'NONE',  ( 0.000000000000000000, 0.000000000000000000, 25.00000000000000000 ) ) ;
#13616 = CARTESIAN_POINT ( 'NONE',  ( 10.00000000000000000, -90.63195040374174027, -18.50093422002511900 ) ) ;
#13618 = CIRCLE ( 'NONE', #12197, 0.02569999999999482421 ) ;
#13617 = LINE ( 'NONE', #20479, #21802 ) ;
#13619 = ORIENTED_EDGE ( 'NONE', *, *, #2414, .F. ) ;
#13620 = ADVANCED_FACE ( 'NONE', ( #10163 ), #3316, .F. ) ;
#13621 = CARTESIAN_POINT ( 'NONE',  ( 10.00000000000000000, 21.65267340503250537, 89.93106657554442052 ) ) ;
#13622 =( REPRESENTATION_RELATIONSHIP ('NONE','NONE', #2177, #10365 ) REPRESENTATION_RELATIONSHIP_WITH_TRANSFORMATION ( #5219 )SHAPE_REPRESENTATION_RELATIONSHIP( ) );
#13623 = CARTESIAN_POINT ( 'NONE',  ( 10.00000000000000000, 0.000000000000000000, 0.000000000000000000 ) ) ;
#13624 = ORIENTED_EDGE ( 'NONE', *, *, #2444, .F. ) ;
#13625 = AXIS2_PLACEMENT_3D ( 'NONE', #9943, #5208, #15240 ) ;
#13626 = CARTESIAN_POINT ( 'NONE',  ( 0.000000000000000000, 0.000000000000000000, 0.000000000000000000 ) ) ;
#13627 = VERTEX_POINT ( 'NONE', #15027 ) ;
#13628 = AXIS2_PLACEMENT_3D ( 'NONE', #15371, #15489, #18484 ) ;
#13629 = ORIENTED_EDGE ( 'NONE', *, *, #716, .F. ) ;
#13630 = CARTESIAN_POINT ( 'NONE',  ( 10.00000000000000000, 83.35585896458619004, 16.94078559807978124 ) ) ;
#13631 = ORIENTED_EDGE ( 'NONE', *, *, #14344, .F. ) ;
#13632 = EDGE_LOOP ( 'NONE', ( #7039, #16214, #16841, #20042 ) ) ;
#13633 = CARTESIAN_POINT ( 'NONE',  ( 10.00000000000000000, -30.24235385705245349, 10.45944707835097098 ) ) ;
#13634 = DIRECTION ( 'NONE',  ( 0.000000000000000000, 1.000000000000000000, -1.224646799147353207E-16 ) ) ;
#13635 = LINE ( 'NONE', #10217, #18534 ) ;
#13636 = DIRECTION ( 'NONE',  ( 0.000000000000000000, -1.000000000000000000, 0.000000000000000000 ) ) ;
#13637 = EDGE_CURVE ( 'NONE', #2166, #610, #18785, .T. ) ;
#13638 = ADVANCED_FACE ( 'NONE', ( #1665 ), #3539, .T. ) ;
#13639 = CARTESIAN_POINT ( 'NONE',  ( 10.00000000000000000, -10.41137886060045226, -91.91321010181856366 ) ) ;
#13640 = EDGE_CURVE ( 'NONE', #1439, #21814, #5205, .T. ) ;
#13641 = DIRECTION ( 'NONE',  ( -1.000000000000000000, -0.000000000000000000, -0.000000000000000000 ) ) ;
#13642 = LINE ( 'NONE', #5360, #5062 ) ;
#13643 = CYLINDRICAL_SURFACE ( 'NONE', #15124, 45.00000000000000000 ) ;
#13644 = EDGE_CURVE ( 'NONE', #21459, #19543, #9064, .T. ) ;
#13645 = AXIS2_PLACEMENT_3D ( 'NONE', #8495, #1645, #20103 ) ;
#13646 = ORIENTED_EDGE ( 'NONE', *, *, #6640, .T. ) ;
#13647 = CIRCLE ( 'NONE', #13994, 44.99999999999999289 ) ;
#13648 = CYLINDRICAL_SURFACE ( 'NONE', #11991, 44.99999999999999289 ) ;
#13649 = LINE ( 'NONE', #19134, #18902 ) ;
#13650 = VERTEX_POINT ( 'NONE', #12042 ) ;
#13651 = CARTESIAN_POINT ( 'NONE',  ( 10.00000000000000000, 0.000000000000000000, 0.000000000000000000 ) ) ;
#13652 = ADVANCED_FACE ( 'NONE', ( #13470 ), #6651, .F. ) ;
#13653 = ORIENTED_EDGE ( 'NONE', *, *, #11948, .T. ) ;
#13654 = DIRECTION ( 'NONE',  ( 0.000000000000000000, 0.000000000000000000, 1.000000000000000000 ) ) ;
#13655 = CARTESIAN_POINT ( 'NONE',  ( 0.000000000000000000, -24.17932380791732427, 20.96092317126997884 ) ) ;
#13656 = EDGE_LOOP ( 'NONE', ( #519, #3554, #11782, #3396 ) ) ;
#13657 = LINE ( 'NONE', #18429, #14495 ) ;
#13658 = EDGE_CURVE ( 'NONE', #20618, #9731, #18576, .T. ) ;
#13659 = AXIS2_PLACEMENT_3D ( 'NONE', #3317, #16471, #11501 ) ;
#13660 = EDGE_LOOP ( 'NONE', ( #11659, #11157, #19577, #15661 ) ) ;
#13661 = VERTEX_POINT ( 'NONE', #10271 ) ;
#13662 = AXIS2_PLACEMENT_3D ( 'NONE', #19411, #16094, #958 ) ;
#13663 = ORIENTED_EDGE ( 'NONE', *, *, #4878, .T. ) ;
#13664 = DIRECTION ( 'NONE',  ( 1.000000000000000000, 0.000000000000000000, 0.000000000000000000 ) ) ;
#13665 = AXIS2_PLACEMENT_3D ( 'NONE', #20452, #8511, #10373 ) ;
#13666 = VERTEX_POINT ( 'NONE', #18462 ) ;
#13667 = CYLINDRICAL_SURFACE ( 'NONE', #20104, 32.00000000000000000 ) ;
#13668 = DIRECTION ( 'NONE',  ( 0.000000000000000000, 0.8660254037844362651, 0.5000000000000041078 ) ) ;
#13669 = FACE_OUTER_BOUND ( 'NONE', #2837, .T. ) ;
#13670 = CARTESIAN_POINT ( 'NONE',  ( -10.00000000000000000, 0.000000000000000000, 0.000000000000000000 ) ) ;
#13671 = CARTESIAN_POINT ( 'NONE',  ( 5.000000000000000888, -6.063030049135288202, 31.42037024962122871 ) ) ;
#13672 = DIRECTION ( 'NONE',  ( 0.000000000000000000, 0.000000000000000000, 1.000000000000000000 ) ) ;
#13673 = EDGE_CURVE ( 'NONE', #7456, #19336, #17129, .T. ) ;
#13674 = DIRECTION ( 'NONE',  ( 1.000000000000000000, 0.000000000000000000, 0.000000000000000000 ) ) ;
#13675 = DIRECTION ( 'NONE',  ( 0.000000000000000000, 0.000000000000000000, 1.000000000000000000 ) ) ;
#13676 = CARTESIAN_POINT ( 'NONE',  ( 10.00000000000000000, 0.000000000000000000, 0.000000000000000000 ) ) ;
#13677 = VECTOR ( 'NONE', #7371, 1000.000000000000000 ) ;
#13678 = FACE_OUTER_BOUND ( 'NONE', #12697, .T. ) ;
#13679 = CIRCLE ( 'NONE', #9785, 44.99999999999999289 ) ;
#13680 = CIRCLE ( 'NONE', #6287, 88.00000000000000000 ) ;
#13681 = CARTESIAN_POINT ( 'NONE',  ( 0.000000000000000000, 28.00896854772012645, -15.47571261340896065 ) ) ;
#13682 = EDGE_CURVE ( 'NONE', #10824, #18424, #5087, .T. ) ;
#13683 = VERTEX_POINT ( 'NONE', #21767 ) ;
#13684 = CARTESIAN_POINT ( 'NONE',  ( 7.440711023145602176, 0.000000000000000000, 0.000000000000000000 ) ) ;
#13685 = VERTEX_POINT ( 'NONE', #227 ) ;
#13686 = CYLINDRICAL_SURFACE ( 'NONE', #13710, 11.99999999999999822 ) ;
#13687 = EDGE_CURVE ( 'NONE', #18956, #6087, #7317, .T. ) ;
#13688 = ORIENTED_EDGE ( 'NONE', *, *, #1097, .F. ) ;
#13689 = EDGE_LOOP ( 'NONE', ( #8500, #16872, #7189, #9265 ) ) ;
#13690 = ADVANCED_FACE ( 'NONE', ( #20343 ), #11937, .T. ) ;
#13691 = EDGE_CURVE ( 'NONE', #14453, #2130, #8730, .T. ) ;
#13692 = VERTEX_POINT ( 'NONE', #11713 ) ;
#13693 = CARTESIAN_POINT ( 'NONE',  ( 1.199999999999998845, 6.728125000000023448, 0.000000000000000000 ) ) ;
#13694 = AXIS2_PLACEMENT_3D ( 'NONE', #11518, #20359, #18378 ) ;
#13695 = CIRCLE ( 'NONE', #17234, 92.50099999999999056 ) ;
#13696 = ORIENTED_EDGE ( 'NONE', *, *, #5997, .F. ) ;
#13697 = CARTESIAN_POINT ( 'NONE',  ( 0.000000000000000000, 0.000000000000000000, 0.000000000000000000 ) ) ;
#13698 = AXIS2_PLACEMENT_3D ( 'NONE', #21486, #7111, #20582 ) ;
#13699 = CIRCLE ( 'NONE', #2040, 44.99999999999999289 ) ;
#13700 = VECTOR ( 'NONE', #3232, 1000.000000000000000 ) ;
#13701 = CARTESIAN_POINT ( 'NONE',  ( 10.00000000000000000, 0.000000000000000000, 0.000000000000000000 ) ) ;
#13702 = DIRECTION ( 'NONE',  ( -1.000000000000000000, 0.000000000000000000, -0.000000000000000000 ) ) ;
#13703 = CYLINDRICAL_SURFACE ( 'NONE', #11184, 11.99999999999999822 ) ;
#13704 = FACE_OUTER_BOUND ( 'NONE', #20885, .T. ) ;
#13705 = CARTESIAN_POINT ( 'NONE',  ( 10.00000000000000000, 16.79755869217770936, -90.96305306542237190 ) ) ;
#13706 = CYLINDRICAL_SURFACE ( 'NONE', #20444, 44.99999999999998579 ) ;
#13707 = EDGE_LOOP ( 'NONE', ( #16058, #1504, #20263, #263 ) ) ;
#13708 = DIRECTION ( 'NONE',  ( 0.000000000000000000, 0.000000000000000000, 1.000000000000000000 ) ) ;
#13709 = AXIS2_PLACEMENT_3D ( 'NONE', #6641, #9823, #16792 ) ;
#13710 = AXIS2_PLACEMENT_3D ( 'NONE', #5620, #7163, #20753 ) ;
#13711 = ORIENTED_EDGE ( 'NONE', *, *, #5326, .T. ) ;
#13712 = AXIS2_PLACEMENT_3D ( 'NONE', #20007, #1223, #11164 ) ;
#13713 = CIRCLE ( 'NONE', #19002, 92.50100000000000477 ) ;
#13714 = AXIS2_PLACEMENT_3D ( 'NONE', #443, #2105, #16801 ) ;
#13715 = VERTEX_POINT ( 'NONE', #17348 ) ;
#13716 = CARTESIAN_POINT ( 'NONE',  ( 10.00000000000000000, 79.38136668499790005, -37.98155635597233726 ) ) ;
#13717 = ORIENTED_EDGE ( 'NONE', *, *, #18162, .T. ) ;
#13718 = ORIENTED_EDGE ( 'NONE', *, *, #11441, .F. ) ;
#13719 = CARTESIAN_POINT ( 'NONE',  ( 0.000000000000000000, 29.29369617358468858, 87.74003855418408193 ) ) ;
#13720 = VERTEX_POINT ( 'NONE', #10599 ) ;
#13721 = CIRCLE ( 'NONE', #21137, 88.00000000000000000 ) ;
#13722 = DIRECTION ( 'NONE',  ( -1.000000000000000000, 0.000000000000000000, 0.000000000000000000 ) ) ;
#13723 = AXIS2_PLACEMENT_3D ( 'NONE', #1082, #14124, #6177 ) ;
#13724 = CARTESIAN_POINT ( 'NONE',  ( 5.000000000000000000, 87.44637528609661103, 9.855528870798920593 ) ) ;
#13725 = DIRECTION ( 'NONE',  ( -1.000000000000000000, -0.000000000000000000, 0.000000000000000000 ) ) ;
#13726 = VECTOR ( 'NONE', #10331, 1000.000000000000000 ) ;
#13727 = DIRECTION ( 'NONE',  ( -1.000000000000000000, 0.000000000000000000, 0.000000000000000000 ) ) ;
#13728 = AXIS2_PLACEMENT_3D ( 'NONE', #18768, #21752, #20208 ) ;
#13729 = VECTOR ( 'NONE', #17570, 1000.000000000000000 ) ;
#13730 = DIRECTION ( 'NONE',  ( 0.000000000000000000, 0.9848077530122073542, 0.1736481776669339672 ) ) ;
#13731 = CARTESIAN_POINT ( 'NONE',  ( 10.00000000000000000, -51.76708072107932423, 67.49339815138475274 ) ) ;
#13732 = DIRECTION ( 'NONE',  ( -1.000000000000000000, -0.000000000000000000, -0.000000000000000000 ) ) ;
#13733 = ORIENTED_EDGE ( 'NONE', *, *, #9308, .T. ) ;
#13734 = CARTESIAN_POINT ( 'NONE',  ( 0.000000000000000000, -85.22372865846305956, 21.92979875759597874 ) ) ;
#13735 = AXIS2_PLACEMENT_3D ( 'NONE', #304, #1844, #18540 ) ;
#13736 = CARTESIAN_POINT ( 'NONE',  ( 10.00000000000000000, 0.000000000000000000, 0.000000000000000000 ) ) ;
#13737 = ORIENTED_EDGE ( 'NONE', *, *, #20708, .F. ) ;
#13738 = EDGE_CURVE ( 'NONE', #1178, #879, #6617, .T. ) ;
#13739 = CIRCLE ( 'NONE', #3160, 92.50100000000000477 ) ;
#13740 = CIRCLE ( 'NONE', #15859, 12.00000000000000000 ) ;
#13741 = CARTESIAN_POINT ( 'NONE',  ( -2.799999999999996714, 60.00000000000000000, -15.00000000000000000 ) ) ;
#13743 = AXIS2_PLACEMENT_3D ( 'NONE', #3296, #15649, #14324 ) ;
#13742 = PRODUCT_DEFINITION_SHAPE ( 'NONE', 'NONE',  #5916 ) ;
#13744 = ORIENTED_EDGE ( 'NONE', *, *, #10944, .T. ) ;
#13745 = PRESENTATION_STYLE_ASSIGNMENT (( #3900 ) ) ;
#13746 = ORIENTED_EDGE ( 'NONE', *, *, #17703, .T. ) ;
#13747 = CARTESIAN_POINT ( 'NONE',  ( 0.000000000000000000, 0.000000000000000000, 0.000000000000000000 ) ) ;
#13748 = ORIENTED_EDGE ( 'NONE', *, *, #9749, .F. ) ;
#13749 = ORIENTED_EDGE ( 'NONE', *, *, #6514, .T. ) ;
#13750 = CARTESIAN_POINT ( 'NONE',  ( 10.00000000000000000, 0.000000000000000000, 0.000000000000000000 ) ) ;
#13751 = CARTESIAN_POINT ( 'NONE',  ( 0.000000000000000000, 0.000000000000000000, 0.000000000000000000 ) ) ;
#13752 = EDGE_CURVE ( 'NONE', #10259, #5155, #16121, .T. ) ;
#13753 = CARTESIAN_POINT ( 'NONE',  ( 8.000000000000007105, 1.284654492305574008E-14, 104.9000000000000341 ) ) ;
#13754 = DIRECTION ( 'NONE',  ( 0.000000000000000000, 0.000000000000000000, -1.000000000000000000 ) ) ;
#13755 = DIRECTION ( 'NONE',  ( -1.000000000000000000, -0.000000000000000000, -0.000000000000000000 ) ) ;
#13756 = CYLINDRICAL_SURFACE ( 'NONE', #11804, 104.9000000000000341 ) ;
#13757 = DIRECTION ( 'NONE',  ( 1.000000000000000000, 0.000000000000000000, 0.000000000000000000 ) ) ;
#13758 = DIRECTION ( 'NONE',  ( 1.000000000000000000, -0.000000000000000000, -0.000000000000000000 ) ) ;
#13759 = AXIS2_PLACEMENT_3D ( 'NONE', #18396, #9873, #3138 ) ;
#13760 = ORIENTED_EDGE ( 'NONE', *, *, #3376, .T. ) ;
#13761 = CARTESIAN_POINT ( 'NONE',  ( 0.000000000000000000, 0.000000000000000000, 15.00000000000000000 ) ) ;
#13762 = CARTESIAN_POINT ( 'NONE',  ( 10.00000000000000000, 66.01871308925461790, 64.79170103523043167 ) ) ;
#13763 = ORIENTED_EDGE ( 'NONE', *, *, #7548, .T. ) ;
#13764 = DIRECTION ( 'NONE',  ( 1.000000000000000000, 0.000000000000000000, 0.000000000000000000 ) ) ;
#13765 = ORIENTED_EDGE ( 'NONE', *, *, #16081, .T. ) ;
#13766 = DIRECTION ( 'NONE',  ( 0.000000000000000000, 0.5877852522924690293, 0.8090169943749504489 ) ) ;
#13767 = EDGE_CURVE ( 'NONE', #20636, #20241, #20718, .T. ) ;
#13768 = EDGE_CURVE ( 'NONE', #18065, #13052, #257, .T. ) ;
#13769 = CARTESIAN_POINT ( 'NONE',  ( 10.00000000000000000, 0.000000000000000000, 0.000000000000000000 ) ) ;
#13770 = VERTEX_POINT ( 'NONE', #17672 ) ;
#13771 =( LENGTH_UNIT ( ) NAMED_UNIT ( * ) SI_UNIT ( .MILLI., .METRE. ) );
#13772 = VERTEX_POINT ( 'NONE', #19211 ) ;
#13773 = ORIENTED_EDGE ( 'NONE', *, *, #16640, .F. ) ;
#13774 = EDGE_LOOP ( 'NONE', ( #7658, #9637, #12475, #12826 ) ) ;
#13775 = AXIS2_PLACEMENT_3D ( 'NONE', #9394, #2890, #2670 ) ;
#13776 = DIRECTION ( 'NONE',  ( 1.000000000000000000, 0.000000000000000000, 0.000000000000000000 ) ) ;
#13777 = EDGE_LOOP ( 'NONE', ( #7920, #12750, #19930, #3177 ) ) ;
#13778 = CARTESIAN_POINT ( 'NONE',  ( 10.00000000000000000, 0.000000000000000000, 0.000000000000000000 ) ) ;
#13779 = DIRECTION ( 'NONE',  ( 1.000000000000000000, 0.000000000000000000, 0.000000000000000000 ) ) ;
#13780 = CARTESIAN_POINT ( 'NONE',  ( 10.00000000000000000, 70.37753541435941429, 60.02863908169658202 ) ) ;
#13781 = FACE_OUTER_BOUND ( 'NONE', #4019, .T. ) ;
#13782 = CARTESIAN_POINT ( 'NONE',  ( 0.000000000000000000, 0.000000000000000000, 0.000000000000000000 ) ) ;
#13783 = DIRECTION ( 'NONE',  ( -1.000000000000000000, -0.000000000000000000, 0.000000000000000000 ) ) ;
#13784 = EDGE_CURVE ( 'NONE', #3730, #17431, #15788, .T. ) ;
#13785 = CARTESIAN_POINT ( 'NONE',  ( 10.00000000000000000, 27.40684453873966575, 16.51862198942017557 ) ) ;
#13786 = DIRECTION ( 'NONE',  ( -1.000000000000000000, -0.000000000000000000, 0.000000000000000000 ) ) ;
#13787 = ORIENTED_EDGE ( 'NONE', *, *, #11078, .T. ) ;
#13788 = EDGE_CURVE ( 'NONE', #2262, #8340, #5741, .T. ) ;
#13789 = DIRECTION ( 'NONE',  ( 0.000000000000000000, 0.9993908270190958731, -0.03489949670249761771 ) ) ;
#13790 = CARTESIAN_POINT ( 'NONE',  ( 120.0000000000000000, 0.000000000000000000, 0.000000000000000000 ) ) ;
#13791 = AXIS2_PLACEMENT_3D ( 'NONE', #15585, #3651, #17468 ) ;
#13792 = CARTESIAN_POINT ( 'NONE',  ( 10.00000000000000000, 0.000000000000000000, 0.000000000000000000 ) ) ;
#13793 = ORIENTED_EDGE ( 'NONE', *, *, #5829, .T. ) ;
#13794 = EDGE_CURVE ( 'NONE', #10604, #3544, #6271, .T. ) ;
#13795 = SURFACE_STYLE_FILL_AREA ( #1647 ) ;
#13796 = ADVANCED_FACE ( 'NONE', ( #13909 ), #5635, .F. ) ;
#13797 = EDGE_CURVE ( 'NONE', #18170, #10147, #9152, .T. ) ;
#13798 = VERTEX_POINT ( 'NONE', #759 ) ;
#13799 = CARTESIAN_POINT ( 'NONE',  ( 0.000000000000000000, 18.94217447942673971, -85.93715160505934136 ) ) ;
#13800 = ORIENTED_EDGE ( 'NONE', *, *, #16610, .T. ) ;
#13801 = EDGE_CURVE ( 'NONE', #9924, #15910, #1667, .T. ) ;
#13802 = EDGE_LOOP ( 'NONE', ( #21842, #191, #9015, #16008 ) ) ;
#13803 = ORIENTED_EDGE ( 'NONE', *, *, #3398, .T. ) ;
#13804 = DIRECTION ( 'NONE',  ( 0.000000000000000000, 0.9702957262759954737, 0.2419218955996715048 ) ) ;
#13805 = DIRECTION ( 'NONE',  ( -1.000000000000000000, -0.000000000000000000, 0.000000000000000000 ) ) ;
#13806 = CARTESIAN_POINT ( 'NONE',  ( 0.000000000000000000, -17.70753755129051754, 21.03896658273966480 ) ) ;
#13807 = CARTESIAN_POINT ( 'NONE',  ( 150.0000507999999968, 3.673940397442060361E-16, -3.000000000000000444 ) ) ;
#13808 = EDGE_CURVE ( 'NONE', #18737, #616, #16831, .T. ) ;
#13809 = DIRECTION ( 'NONE',  ( 0.000000000000000000, 0.000000000000000000, 1.000000000000000000 ) ) ;
#13810 = CARTESIAN_POINT ( 'NONE',  ( 10.00000000000000000, -84.80486432185169576, -36.94008646920480743 ) ) ;
#13811 = FACE_OUTER_BOUND ( 'NONE', #7688, .T. ) ;
#13812 = ADVANCED_FACE ( 'NONE', ( #2309 ), #20655, .F. ) ;
#13813 = CARTESIAN_POINT ( 'NONE',  ( -8.000000000000007105, 0.000000000000000000, 0.000000000000000000 ) ) ;
#13814 = DIRECTION ( 'NONE',  ( 1.000000000000000000, 0.000000000000000000, 0.000000000000000000 ) ) ;
#13815 = ORIENTED_EDGE ( 'NONE', *, *, #1661, .F. ) ;
#13816 = EDGE_CURVE ( 'NONE', #9731, #7352, #18605, .T. ) ;
#13817 = CARTESIAN_POINT ( 'NONE',  ( 10.00000000000000000, 4.294029059349855793, 27.86182539015968018 ) ) ;
#13818 = AXIS2_PLACEMENT_3D ( 'NONE', #8985, #3810, #10542 ) ;
#13819 = VERTEX_POINT ( 'NONE', #4190 ) ;
#13820 = ORIENTED_EDGE ( 'NONE', *, *, #13392, .T. ) ;
#13821 = DIRECTION ( 'NONE',  ( 0.000000000000000000, -0.9945218953682744001, 0.1045284632676437425 ) ) ;
#13822 = ADVANCED_FACE ( 'NONE', ( #12364 ), #655, .F. ) ;
#13823 = ORIENTED_EDGE ( 'NONE', *, *, #9598, .F. ) ;
#13824 = VERTEX_POINT ( 'NONE', #550 ) ;
#13825 = CARTESIAN_POINT ( 'NONE',  ( 0.000000000000000000, 0.000000000000000000, 0.000000000000000000 ) ) ;
#13826 = ORIENTED_EDGE ( 'NONE', *, *, #10268, .F. ) ;
#13827 = DIRECTION ( 'NONE',  ( 1.000000000000000000, 0.000000000000000000, 0.000000000000000000 ) ) ;
#13828 = DIRECTION ( 'NONE',  ( 0.000000000000000000, 0.000000000000000000, 1.000000000000000000 ) ) ;
#13829 = DIRECTION ( 'NONE',  ( 0.000000000000000000, 0.9702957262759972501, -0.2419218955996647880 ) ) ;
#13830 = CARTESIAN_POINT ( 'NONE',  ( 10.00000000000000000, 0.000000000000000000, 0.000000000000000000 ) ) ;
#13831 = EDGE_CURVE ( 'NONE', #18291, #4269, #19427, .T. ) ;
#13832 = LINE ( 'NONE', #3341, #6851 ) ;
#13833 = CARTESIAN_POINT ( 'NONE',  ( 5.000000000000000000, 67.00000000000000000, 15.00000000000000000 ) ) ;
#13834 = CARTESIAN_POINT ( 'NONE',  ( 9.999999999999998224, 1.224646799147353059E-15, 15.00000000000000000 ) ) ;
#13835 = EDGE_LOOP ( 'NONE', ( #3111, #5480, #14990, #15905 ) ) ;
#13836 = EDGE_CURVE ( 'NONE', #750, #21012, #10832, .T. ) ;
#13837 = VECTOR ( 'NONE', #8555, 1000.000000000000000 ) ;
#13838 = DIRECTION ( 'NONE',  ( -1.000000000000000000, 0.000000000000000000, 0.000000000000000000 ) ) ;
#13839 = CYLINDRICAL_SURFACE ( 'NONE', #14106, 27.49900000000000233 ) ;
#13840 = ORIENTED_EDGE ( 'NONE', *, *, #6132, .F. ) ;
#13841 = DIRECTION ( 'NONE',  ( 0.000000000000000000, 0.8660254037844361541, 0.5000000000000041078 ) ) ;
#13842 = ORIENTED_EDGE ( 'NONE', *, *, #7062, .T. ) ;
#13843 = SHAPE_REPRESENTATION_RELATIONSHIP ( 'NONE' , 'NONE' ,  #10365, #4298 ) ;
#13844 = DIRECTION ( 'NONE',  ( 0.000000000000000000, -0.06975647374411138302, -0.9975640502598251969 ) ) ;
#13845 = AXIS2_PLACEMENT_3D ( 'NONE', #11045, #12806, #21115 ) ;
#13846 = VERTEX_POINT ( 'NONE', #19109 ) ;
#13847 = ORIENTED_EDGE ( 'NONE', *, *, #14050, .F. ) ;
#13848 = PLANE ( 'NONE',  #19915 ) ;
#13849 = CYLINDRICAL_SURFACE ( 'NONE', #14546, 44.99999999999998579 ) ;
#13850 = CIRCLE ( 'NONE', #14560, 126.5000000000000000 ) ;
#13851 = CYLINDRICAL_SURFACE ( 'NONE', #16753, 92.50100000000000477 ) ;
#13852 = CARTESIAN_POINT ( 'NONE',  ( 10.00000000000000000, -3.974475837765555575, 92.41557521768190497 ) ) ;
#13853 = DIRECTION ( 'NONE',  ( -1.000000000000000000, -0.000000000000000000, 0.000000000000000000 ) ) ;
#13854 = CARTESIAN_POINT ( 'NONE',  ( 10.00000000000000000, 25.56104204395415991, -81.12843256239638379 ) ) ;
#13855 = EDGE_CURVE ( 'NONE', #16620, #6035, #2009, .T. ) ;
#13856 = CIRCLE ( 'NONE', #14914, 44.99999999999999289 ) ;
#13857 = DIRECTION ( 'NONE',  ( -1.000000000000000000, 0.000000000000000000, 0.000000000000000000 ) ) ;
#13858 = CYLINDRICAL_SURFACE ( 'NONE', #17252, 88.00000000000000000 ) ;
#13859 = ORIENTED_EDGE ( 'NONE', *, *, #13564, .T. ) ;
#13860 = DIRECTION ( 'NONE',  ( 0.000000000000000000, 0.000000000000000000, -1.000000000000000000 ) ) ;
#13861 = AXIS2_PLACEMENT_3D ( 'NONE', #3861, #20450, #225 ) ;
#13862 = ORIENTED_EDGE ( 'NONE', *, *, #15134, .T. ) ;
#13863 = DIRECTION ( 'NONE',  ( -1.000000000000000000, -0.000000000000000000, -0.000000000000000000 ) ) ;
#13864 = ORIENTED_EDGE ( 'NONE', *, *, #9080, .T. ) ;
#13865 = AXIS2_PLACEMENT_3D ( 'NONE', #758, #12464, #20551 ) ;
#13866 = DIRECTION ( 'NONE',  ( -1.000000000000000000, -0.000000000000000000, -0.000000000000000000 ) ) ;
#13867 = DIRECTION ( 'NONE',  ( 0.000000000000000000, 0.000000000000000000, 1.000000000000000000 ) ) ;
#13868 = VERTEX_POINT ( 'NONE', #8166 ) ;
#13869 = CIRCLE ( 'NONE', #17758, 92.50099999999999056 ) ;
#13870 = ORIENTED_EDGE ( 'NONE', *, *, #6556, .F. ) ;
#13871 = ORIENTED_EDGE ( 'NONE', *, *, #3681, .F. ) ;
#13872 = EDGE_LOOP ( 'NONE', ( #8889, #14027, #9602, #1300 ) ) ;
#13873 = DIRECTION ( 'NONE',  ( 1.000000000000000000, -0.000000000000000000, -0.000000000000000000 ) ) ;
#13874 = VERTEX_POINT ( 'NONE', #12785 ) ;
#13875 = CARTESIAN_POINT ( 'NONE',  ( 10.00000000000000000, 0.000000000000000000, 0.000000000000000000 ) ) ;
#13876 = CARTESIAN_POINT ( 'NONE',  ( -2.000000000000000000, 70.00000000000000000, 15.00000000000000000 ) ) ;
#13877 = CARTESIAN_POINT ( 'NONE',  ( 10.00000000000000000, 52.34334029047981574, -76.26670130689429072 ) ) ;
#13878 = CARTESIAN_POINT ( 'NONE',  ( 10.00000000000000000, -61.60362715318993310, -62.84101464466307618 ) ) ;
#13879 = CARTESIAN_POINT ( 'NONE',  ( 0.000000000000000000, 27.07404830566976983, -4.815694066514164540 ) ) ;
#13880 = VECTOR ( 'NONE', #13857, 1000.000000000000000 ) ;
#13881 = EDGE_CURVE ( 'NONE', #9164, #5724, #17550, .T. ) ;
#13882 = DIRECTION ( 'NONE',  ( -1.000000000000000000, 0.000000000000000000, 0.000000000000000000 ) ) ;
#13883 = EDGE_LOOP ( 'NONE', ( #2640, #3955, #3653, #4891 ) ) ;
#13884 = AXIS2_PLACEMENT_3D ( 'NONE', #20087, #15539, #2065 ) ;
#13885 = LINE ( 'NONE', #2392, #16938 ) ;
#13886 = AXIS2_PLACEMENT_3D ( 'NONE', #2012, #247, #8533 ) ;
#13887 = DIRECTION ( 'NONE',  ( 0.000000000000000000, 0.000000000000000000, -1.000000000000000000 ) ) ;
#13888 = EDGE_CURVE ( 'NONE', #13385, #20271, #20374, .T. ) ;
#13889 = CARTESIAN_POINT ( 'NONE',  ( 0.000000000000000000, 0.000000000000000000, 0.000000000000000000 ) ) ;
#13890 = VERTEX_POINT ( 'NONE', #7727 ) ;
#13891 = AXIS2_PLACEMENT_3D ( 'NONE', #16084, #2831, #12761 ) ;
#13892 = CYLINDRICAL_SURFACE ( 'NONE', #19016, 88.00000000000000000 ) ;
#13893 = VERTEX_POINT ( 'NONE', #11587 ) ;
#13894 = CARTESIAN_POINT ( 'NONE',  ( 0.000000000000000000, -30.24235385705231849, -10.45944707835137777 ) ) ;
#13895 = ORIENTED_EDGE ( 'NONE', *, *, #15927, .T. ) ;
#13896 = EDGE_CURVE ( 'NONE', #20086, #13770, #18954, .T. ) ;
#13897 = AXIS2_PLACEMENT_3D ( 'NONE', #20922, #5577, #17722 ) ;
#13898 = ORIENTED_EDGE ( 'NONE', *, *, #10165, .T. ) ;
#13899 = AXIS2_PLACEMENT_3D ( 'NONE', #6374, #12979, #6148 ) ;
#13900 = ORIENTED_EDGE ( 'NONE', *, *, #4346, .F. ) ;
#13901 = CARTESIAN_POINT ( 'NONE',  ( -90.00000000000000000, 0.000000000000000000, 0.000000000000000000 ) ) ;
#13902 = LINE ( 'NONE', #19914, #19220 ) ;
#13903 = LINE ( 'NONE', #7399, #11389 ) ;
#13904 = LINE ( 'NONE', #13807, #20570 ) ;
#13905 = AXIS2_PLACEMENT_3D ( 'NONE', #20599, #15188, #3588 ) ;
#13906 = EDGE_CURVE ( 'NONE', #20618, #19098, #19308, .T. ) ;
#13907 = FACE_OUTER_BOUND ( 'NONE', #16132, .T. ) ;
#13908 = ADVANCED_FACE ( 'NONE', ( #16114 ), #11353, .T. ) ;
#13909 = FACE_OUTER_BOUND ( 'NONE', #7092, .T. ) ;
#13910 = DIRECTION ( 'NONE',  ( -1.000000000000000000, 0.000000000000000000, 0.000000000000000000 ) ) ;
#13911 = ADVANCED_FACE ( 'NONE', ( #19652 ), #21304, .T. ) ;
#13912 = CARTESIAN_POINT ( 'NONE',  ( 123.5000000000000142, 0.000000000000000000, 0.000000000000000000 ) ) ;
#13913 = FACE_OUTER_BOUND ( 'NONE', #10625, .T. ) ;
#13914 = AXIS2_PLACEMENT_3D ( 'NONE', #20195, #8484, #7051 ) ;
#13915 = EDGE_CURVE ( 'NONE', #5097, #9782, #2750, .T. ) ;
#13916 = EDGE_LOOP ( 'NONE', ( #9678, #9030, #13479, #2622 ) ) ;
#13917 = AXIS2_PLACEMENT_3D ( 'NONE', #21247, #2899, #17825 ) ;
#13918 = CARTESIAN_POINT ( 'NONE',  ( 0.000000000000000000, 0.000000000000000000, 3.000000000000002665 ) ) ;
#13919 = ORIENTED_EDGE ( 'NONE', *, *, #5461, .F. ) ;
#13920 = EDGE_LOOP ( 'NONE', ( #18746, #8360, #18587, #9725 ) ) ;
#13921 = ORIENTED_EDGE ( 'NONE', *, *, #9361, .F. ) ;
#13922 = EDGE_CURVE ( 'NONE', #16787, #19647, #7655, .T. ) ;
#13923 = CARTESIAN_POINT ( 'NONE',  ( 10.00000000000000000, 81.34229909304679040, 33.57723005635394742 ) ) ;
#13924 = VECTOR ( 'NONE', #16052, 1000.000000000000000 ) ;
#13925 = ORIENTED_EDGE ( 'NONE', *, *, #1748, .F. ) ;
#13926 = AXIS2_PLACEMENT_3D ( 'NONE', #4962, #7945, #21422 ) ;
#13927 = ORIENTED_EDGE ( 'NONE', *, *, #19847, .T. ) ;
#13928 = CIRCLE ( 'NONE', #21688, 88.00000000000000000 ) ;
#13929 = EDGE_CURVE ( 'NONE', #21583, #8568, #13313, .T. ) ;
#13930 = VECTOR ( 'NONE', #6020, 1000.000000000000000 ) ;
#13931 = DIRECTION ( 'NONE',  ( 1.000000000000000000, 0.000000000000000000, 0.000000000000000000 ) ) ;
#13932 = ORIENTED_EDGE ( 'NONE', *, *, #21481, .T. ) ;
#13933 = DIRECTION ( 'NONE',  ( 1.000000000000000000, 0.000000000000000000, 0.000000000000000000 ) ) ;
#13934 = AXIS2_PLACEMENT_3D ( 'NONE', #6676, #18887, #18380 ) ;
#13935 = DIRECTION ( 'NONE',  ( -1.000000000000000000, 0.000000000000000000, -0.000000000000000000 ) ) ;
#13936 = DIRECTION ( 'NONE',  ( -1.000000000000000000, -0.000000000000000000, 0.000000000000000000 ) ) ;
#13937 = DIRECTION ( 'NONE',  ( 0.000000000000000000, 0.000000000000000000, 1.000000000000000000 ) ) ;
#13938 = DIRECTION ( 'NONE',  ( 0.000000000000000000, -8.943463253924875462E-15, -1.000000000000000000 ) ) ;
#13939 = DIRECTION ( 'NONE',  ( 0.000000000000000000, 0.000000000000000000, 1.000000000000000000 ) ) ;
#13940 = DIRECTION ( 'NONE',  ( 0.000000000000000000, 0.000000000000000000, -1.000000000000000000 ) ) ;
#13941 = DIRECTION ( 'NONE',  ( 0.000000000000000000, 0.06975647374411841906, 0.9975640502598247528 ) ) ;
#13942 = EDGE_CURVE ( 'NONE', #10178, #21594, #621, .T. ) ;
#13943 = CIRCLE ( 'NONE', #3359, 7.400000000000019895 ) ;
#13944 = ORIENTED_EDGE ( 'NONE', *, *, #10939, .F. ) ;
#13945 = AXIS2_PLACEMENT_3D ( 'NONE', #3609, #5493, #17095 ) ;
#13946 = VECTOR ( 'NONE', #7204, 1000.000000000000000 ) ;
#13947 = CARTESIAN_POINT ( 'NONE',  ( 10.00000000000000000, 0.000000000000000000, 0.000000000000000000 ) ) ;
#13948 = EDGE_CURVE ( 'NONE', #12492, #9371, #9418, .T. ) ;
#13949 = DIRECTION ( 'NONE',  ( 0.000000000000000000, 0.000000000000000000, 1.000000000000000000 ) ) ;
#13950 = VERTEX_POINT ( 'NONE', #8057 ) ;
#13951 = AXIS2_PLACEMENT_3D ( 'NONE', #20165, #1390, #9981 ) ;
#13952 = DIRECTION ( 'NONE',  ( 1.000000000000000000, 0.000000000000000000, 0.000000000000000000 ) ) ;
#13953 = EDGE_CURVE ( 'NONE', #20112, #1976, #21417, .T. ) ;
#13954 = ORIENTED_EDGE ( 'NONE', *, *, #12851, .T. ) ;
#13955 = SURFACE_STYLE_FILL_AREA ( #5670 ) ;
#13956 = DIRECTION ( 'NONE',  ( 1.000000000000000000, 0.000000000000000000, 0.000000000000000000 ) ) ;
#13957 = EDGE_LOOP ( 'NONE', ( #1436, #18879, #12795, #12803 ) ) ;
#13958 = ORIENTED_EDGE ( 'NONE', *, *, #10536, .T. ) ;
#13959 = EDGE_CURVE ( 'NONE', #8974, #15746, #3076, .T. ) ;
#13960 = CARTESIAN_POINT ( 'NONE',  ( 10.00000000000000000, 27.82509854686817263, -4.525913221810857756 ) ) ;
#13961 = DIRECTION ( 'NONE',  ( -1.000000000000000000, 0.000000000000000000, 0.000000000000000000 ) ) ;
#13962 = CIRCLE ( 'NONE', #10426, 27.49900000000000233 ) ;
#13963 = ADVANCED_FACE ( 'NONE', ( #19765 ), #21200, .T. ) ;
#13964 = VECTOR ( 'NONE', #16252, 1000.000000000000000 ) ;
#13965 = DIRECTION ( 'NONE',  ( 1.000000000000000000, 0.000000000000000000, 0.000000000000000000 ) ) ;
#13966 = CARTESIAN_POINT ( 'NONE',  ( 10.00000000000000000, 14.02138820414913845, 83.89630571862289798 ) ) ;
#13967 = CARTESIAN_POINT ( 'NONE',  ( 0.000000000000000000, 76.53853822673980289, 43.42639941457142072 ) ) ;
#13968 = CARTESIAN_POINT ( 'NONE',  ( 5.000000000000002665, -6.797690662955810481, 87.73705831432212676 ) ) ;
#13969 = CARTESIAN_POINT ( 'NONE',  ( 0.000000000000000000, 0.000000000000000000, 0.000000000000000000 ) ) ;
#13970 = CARTESIAN_POINT ( 'NONE',  ( 7.999999999999979572, 0.000000000000000000, 0.000000000000000000 ) ) ;
#13971 = ORIENTED_EDGE ( 'NONE', *, *, #13518, .T. ) ;
#13972 = AXIS2_PLACEMENT_3D ( 'NONE', #18056, #1258, #21478 ) ;
#13973 = CARTESIAN_POINT ( 'NONE',  ( 1.139999999999998570, 0.000000000000000000, 0.000000000000000000 ) ) ;
#13974 = ORIENTED_EDGE ( 'NONE', *, *, #10402, .T. ) ;
#13975 = AXIS2_PLACEMENT_3D ( 'NONE', #9157, #7947, #14680 ) ;
#13976 =( GEOMETRIC_REPRESENTATION_CONTEXT ( 3 ) GLOBAL_UNCERTAINTY_ASSIGNED_CONTEXT ( ( #16299 ) ) GLOBAL_UNIT_ASSIGNED_CONTEXT ( ( #16383, #16706, #17945 ) ) REPRESENTATION_CONTEXT ( 'NONE', 'WORKASPACE' ) );
#13977 = CARTESIAN_POINT ( 'NONE',  ( 0.000000000000000000, 87.96697768756401103, 2.410567674970879981 ) ) ;
#13978 = ORIENTED_EDGE ( 'NONE', *, *, #12188, .F. ) ;
#13979 = DIRECTION ( 'NONE',  ( 0.000000000000000000, 0.000000000000000000, 1.000000000000000000 ) ) ;
#13980 = DIRECTION ( 'NONE',  ( -1.000000000000000000, -0.000000000000000000, -0.000000000000000000 ) ) ;
#13981 = VERTEX_POINT ( 'NONE', #21535 ) ;
#13982 =( LENGTH_UNIT ( ) NAMED_UNIT ( * ) SI_UNIT ( .MILLI., .METRE. ) );
#13983 = VERTEX_POINT ( 'NONE', #18007 ) ;
#13984 = VERTEX_POINT ( 'NONE', #2858 ) ;
#13985 = ORIENTED_EDGE ( 'NONE', *, *, #2200, .T. ) ;
#13986 = CARTESIAN_POINT ( 'NONE',  ( 10.00000000000000000, -60.65655256511276860, 59.63197188857500919 ) ) ;
#13987 = ORIENTED_EDGE ( 'NONE', *, *, #8165, .F. ) ;
#13988 = CARTESIAN_POINT ( 'NONE',  ( -90.00000000000000000, 9.184850993605175555E-16, 7.500000000000020428 ) ) ;
#13989 = LINE ( 'NONE', #13780, #14751 ) ;
#13990 = AXIS2_PLACEMENT_3D ( 'NONE', #92, #8276, #16667 ) ;
#13991 = CARTESIAN_POINT ( 'NONE',  ( 0.000000000000000000, 62.44821182181091501, 68.23969402963524544 ) ) ;
#13992 = AXIS2_PLACEMENT_3D ( 'NONE', #16024, #12812, #10730 ) ;
#13993 = DIRECTION ( 'NONE',  ( -1.000000000000000000, 0.000000000000000000, 0.000000000000000000 ) ) ;
#13994 = AXIS2_PLACEMENT_3D ( 'NONE', #6327, #11280, #16581 ) ;
#13995 = LINE ( 'NONE', #20740, #18062 ) ;
#13996 = DIRECTION ( 'NONE',  ( 0.000000000000000000, 1.141062553086966690E-14, -1.000000000000000000 ) ) ;
#13997 = VERTEX_POINT ( 'NONE', #9572 ) ;
#13998 = CARTESIAN_POINT ( 'NONE',  ( 0.000000000000000000, 84.80486432185190893, 36.94008646920423899 ) ) ;
#13999 = DIRECTION ( 'NONE',  ( 1.000000000000000000, -0.000000000000000000, -0.000000000000000000 ) ) ;
#14000 = DIRECTION ( 'NONE',  ( -1.000000000000000000, -0.000000000000000000, -0.000000000000000000 ) ) ;
#14001 = ORIENTED_EDGE ( 'NONE', *, *, #16516, .F. ) ;
#14002 = AXIS2_PLACEMENT_3D ( 'NONE', #18134, #21328, #6544 ) ;
#14003 = CARTESIAN_POINT ( 'NONE',  ( 0.000000000000000000, 17.64925110578469258, 86.21197095186350623 ) ) ;
#14004 = AXIS2_PLACEMENT_3D ( 'NONE', #14213, #6055, #14544 ) ;
#14005 = VERTEX_POINT ( 'NONE', #4627 ) ;
#14006 = CARTESIAN_POINT ( 'NONE',  ( 10.00000000000000000, 56.05743251323859511, 67.83483072893820065 ) ) ;
#14007 = AXIS2_PLACEMENT_3D ( 'NONE', #14235, #3967, #15998 ) ;
#14008 = ORIENTED_EDGE ( 'NONE', *, *, #3818, .F. ) ;
#14009 = ORIENTED_EDGE ( 'NONE', *, *, #13241, .T. ) ;
#14010 = ADVANCED_FACE ( 'NONE', ( #21631 ), #18104, .F. ) ;
#14011 = ORIENTED_EDGE ( 'NONE', *, *, #10642, .T. ) ;
#14012 = DIRECTION ( 'NONE',  ( 0.000000000000000000, 0.000000000000000000, 1.000000000000000000 ) ) ;
#14013 = ORIENTED_EDGE ( 'NONE', *, *, #6784, .T. ) ;
#14014 = CARTESIAN_POINT ( 'NONE',  ( -1.129531546211690385, 0.000000000000000000, 0.000000000000000000 ) ) ;
#14015 = DIRECTION ( 'NONE',  ( 1.000000000000000000, 0.000000000000000000, 0.000000000000000000 ) ) ;
#14016 = LINE ( 'NONE', #7080, #10678 ) ;
#14017 = EDGE_CURVE ( 'NONE', #10738, #8155, #965, .T. ) ;
#14018 = DIRECTION ( 'NONE',  ( 0.000000000000000000, -1.000000000000000000, 0.000000000000000000 ) ) ;
#14019 = VECTOR ( 'NONE', #15861, 1000.000000000000000 ) ;
#14020 = DIRECTION ( 'NONE',  ( 1.000000000000000000, 0.000000000000000000, 0.000000000000000000 ) ) ;
#14021 = FACE_OUTER_BOUND ( 'NONE', #10478, .T. ) ;
#14022 = CIRCLE ( 'NONE', #16851, 27.49900000000000233 ) ;
#14023 = FACE_OUTER_BOUND ( 'NONE', #1330, .T. ) ;
#14024 = CYLINDRICAL_SURFACE ( 'NONE', #2432, 88.00000000000000000 ) ;
#14025 = EDGE_LOOP ( 'NONE', ( #127, #21617, #6446, #16599, #20356, #14166 ) ) ;
#14026 = CARTESIAN_POINT ( 'NONE',  ( -1.140000000000000124, 0.000000000000000000, -5.633200000000004870 ) ) ;
#14027 = ORIENTED_EDGE ( 'NONE', *, *, #9840, .F. ) ;
#14028 = ORIENTED_EDGE ( 'NONE', *, *, #13816, .F. ) ;
#14029 = EDGE_LOOP ( 'NONE', ( #5536, #13925 ) ) ;
#14030 = FACE_OUTER_BOUND ( 'NONE', #21342, .T. ) ;
#14031 = ORIENTED_EDGE ( 'NONE', *, *, #16589, .T. ) ;
#14032 = EDGE_CURVE ( 'NONE', #13474, #15205, #17913, .T. ) ;
#14033 = CIRCLE ( 'NONE', #12626, 27.49900000000000233 ) ;
#14034 = ADVANCED_FACE ( 'NONE', ( #10348 ), #3514, .F. ) ;
#14035 = VECTOR ( 'NONE', #3721, 1000.000000000000000 ) ;
#14036 = EDGE_CURVE ( 'NONE', #21192, #2153, #4852, .T. ) ;
#14037 = EDGE_LOOP ( 'NONE', ( #2116, #18447, #14217, #5483 ) ) ;
#14038 = CIRCLE ( 'NONE', #6304, 44.99999999999999289 ) ;
#14039 = DIRECTION ( 'NONE',  ( 0.000000000000000000, 0.1391731009600657432, -0.9902680687415702510 ) ) ;
#14040 = EDGE_CURVE ( 'NONE', #15909, #7517, #6988, .T. ) ;
#14041 = ORIENTED_EDGE ( 'NONE', *, *, #15231, .F. ) ;
#14042 = CARTESIAN_POINT ( 'NONE',  ( 10.00000000000000000, 16.79755869217650144, 90.96305306542258506 ) ) ;
#14043 = CYLINDRICAL_SURFACE ( 'NONE', #18081, 11.99999999999999822 ) ;
#14044 = AXIS2_PLACEMENT_3D ( 'NONE', #20572, #5439, #3776 ) ;
#14045 = FACE_OUTER_BOUND ( 'NONE', #13421, .T. ) ;
#14046 = CARTESIAN_POINT ( 'NONE',  ( 10.00000000000000000, -30.61448696004445580, -9.314139153634537038 ) ) ;
#14047 = CARTESIAN_POINT ( 'NONE',  ( 10.00000000000000000, -21.98203405400967014, 17.64965094506536403 ) ) ;
#14048 = CARTESIAN_POINT ( 'NONE',  ( 0.000000000000000000, 6.063030049135491595, -31.42037024962118608 ) ) ;
#14049 = CARTESIAN_POINT ( 'NONE',  ( 1.500000000000000000, 5.000000000000000000, 7.000000000000000000 ) ) ;
#14050 = EDGE_CURVE ( 'NONE', #6777, #3829, #5555, .T. ) ;
#14051 = DIRECTION ( 'NONE',  ( 0.000000000000000000, 0.7431448254773909134, 0.6691306063588619013 ) ) ;
#14052 = VECTOR ( 'NONE', #2216, 1000.000000000000000 ) ;
#14053 = AXIS2_PLACEMENT_3D ( 'NONE', #2089, #5398, #3740 ) ;
#14054 = AXIS2_PLACEMENT_3D ( 'NONE', #14826, #8194, #1240 ) ;
#14055 = ORIENTED_EDGE ( 'NONE', *, *, #11598, .T. ) ;
#14056 = AXIS2_PLACEMENT_3D ( 'NONE', #6329, #9600, #8187 ) ;
#14057 = EDGE_CURVE ( 'NONE', #6401, #12429, #8386, .T. ) ;
#14058 = CYLINDRICAL_SURFACE ( 'NONE', #2765, 11.99999999999999822 ) ;
#14059 = DIRECTION ( 'NONE',  ( -1.000000000000000000, -0.000000000000000000, -0.000000000000000000 ) ) ;
#14060 = VERTEX_POINT ( 'NONE', #204 ) ;
#14061 = EDGE_CURVE ( 'NONE', #15549, #3324, #15790, .T. ) ;
#14062 = DIRECTION ( 'NONE',  ( 0.000000000000000000, 0.000000000000000000, 1.000000000000000000 ) ) ;
#14063 = VERTEX_POINT ( 'NONE', #13785 ) ;
#14064 =( LENGTH_UNIT ( ) NAMED_UNIT ( * ) SI_UNIT ( .MILLI., .METRE. ) );
#14065 = CIRCLE ( 'NONE', #14787, 0.09999999999999939493 ) ;
#14066 = DIRECTION ( 'NONE',  ( -1.000000000000000000, -0.000000000000000000, -0.000000000000000000 ) ) ;
#14067 = EDGE_CURVE ( 'NONE', #15044, #6894, #5289, .T. ) ;
#14068 = ORIENTED_EDGE ( 'NONE', *, *, #14861, .T. ) ;
#14069 = AXIS2_PLACEMENT_3D ( 'NONE', #16312, #2731, #4276 ) ;
#14070 = ORIENTED_EDGE ( 'NONE', *, *, #10008, .T. ) ;
#14071 = LINE ( 'NONE', #2354, #9677 ) ;
#14072 = VECTOR ( 'NONE', #4172, 1000.000000000000000 ) ;
#14073 = AXIS2_PLACEMENT_3D ( 'NONE', #10053, #16917, #230 ) ;
#14074 = FACE_OUTER_BOUND ( 'NONE', #9073, .T. ) ;
#14075 = DIRECTION ( 'NONE',  ( 1.000000000000000000, -0.000000000000000000, -0.000000000000000000 ) ) ;
#14076 = CARTESIAN_POINT ( 'NONE',  ( 10.00000000000000000, 84.80486432185243473, -36.94008646920313055 ) ) ;
#14077 = CARTESIAN_POINT ( 'NONE',  ( 10.00000000000000000, 0.000000000000000000, 0.000000000000000000 ) ) ;
#14078 = LINE ( 'NONE', #5904, #20247 ) ;
#14079 = DIRECTION ( 'NONE',  ( 1.000000000000000000, 0.000000000000000000, 0.000000000000000000 ) ) ;
#14080 = EDGE_CURVE ( 'NONE', #874, #19022, #8489, .T. ) ;
#14081 = ORIENTED_EDGE ( 'NONE', *, *, #1930, .T. ) ;
#14082 = EDGE_CURVE ( 'NONE', #14609, #10308, #13680, .T. ) ;
#14083 = DIRECTION ( 'NONE',  ( 0.000000000000000000, -0.8660254037844432595, 0.4999999999999918399 ) ) ;
#14084 = CIRCLE ( 'NONE', #11635, 88.00000000000000000 ) ;
#14085 = ORIENTED_EDGE ( 'NONE', *, *, #5269, .F. ) ;
#14086 = EDGE_CURVE ( 'NONE', #8339, #18927, #11695, .T. ) ;
#14087 = CIRCLE ( 'NONE', #21850, 11.99999999999999822 ) ;
#14088 = CIRCLE ( 'NONE', #20110, 45.00000000000000000 ) ;
#14089 = EDGE_CURVE ( 'NONE', #10823, #4316, #13450, .T. ) ;
#14090 = CYLINDRICAL_SURFACE ( 'NONE', #21435, 27.49900000000000233 ) ;
#14091 = VERTEX_POINT ( 'NONE', #6839 ) ;
#14092 = DIRECTION ( 'NONE',  ( 0.000000000000000000, -0.9510565162951502005, -0.3090169943749575543 ) ) ;
#14093 = CYLINDRICAL_SURFACE ( 'NONE', #13029, 5.000000000000000000 ) ;
#14094 = ORIENTED_EDGE ( 'NONE', *, *, #20140, .F. ) ;
#14095 = ORIENTED_EDGE ( 'NONE', *, *, #2553, .T. ) ;
#14096 = EDGE_CURVE ( 'NONE', #19663, #20330, #5925, .T. ) ;
#14097 = EDGE_LOOP ( 'NONE', ( #1622, #18114, #232, #5217 ) ) ;
#14098 = VERTEX_POINT ( 'NONE', #3612 ) ;
#14099 = CARTESIAN_POINT ( 'NONE',  ( 10.00000000000000000, 85.22372865846293166, 21.92979875759657560 ) ) ;
#14100 = DIRECTION ( 'NONE',  ( 0.000000000000000000, 0.6946583704589984753, -0.7193398003386500816 ) ) ;
#14101 = VERTEX_POINT ( 'NONE', #8705 ) ;
#14102 = AXIS2_PLACEMENT_3D ( 'NONE', #19916, #30, #11523 ) ;
#14103 = CARTESIAN_POINT ( 'NONE',  ( 10.00000000000000000, -15.51843147776405729, 83.63233659819645993 ) ) ;
#14104 = DIRECTION ( 'NONE',  ( 1.000000000000000000, 0.000000000000000000, 0.000000000000000000 ) ) ;
#14105 = CARTESIAN_POINT ( 'NONE',  ( 0.000000000000000000, 9.992993448021948666, -26.36019881529875519 ) ) ;
#14106 = AXIS2_PLACEMENT_3D ( 'NONE', #13736, #17277, #9081 ) ;
#14107 = CARTESIAN_POINT ( 'NONE',  ( 0.000000000000000000, -75.45728100697571961, -39.26051685139143643 ) ) ;
#14108 = CARTESIAN_POINT ( 'NONE',  ( 0.000000000000000000, 85.22372865846293166, 21.92979875759657560 ) ) ;
#14109 = ORIENTED_EDGE ( 'NONE', *, *, #1205, .T. ) ;
#14110 = CARTESIAN_POINT ( 'NONE',  ( 7.599999999999998757, 1.408348717606652665E-14, 114.9007999999999896 ) ) ;
#14111 = CARTESIAN_POINT ( 'NONE',  ( 0.000000000000000000, -17.64925110578410639, -86.21197095186363413 ) ) ;
#14112 = EDGE_CURVE ( 'NONE', #10738, #11183, #3293, .T. ) ;
#14113 = DIRECTION ( 'NONE',  ( -1.000000000000000000, -0.000000000000000000, -0.000000000000000000 ) ) ;
#14114 = ORIENTED_EDGE ( 'NONE', *, *, #16407, .T. ) ;
#14115 = DIRECTION ( 'NONE',  ( -1.000000000000000000, -0.000000000000000000, 0.000000000000000000 ) ) ;
#14116 = ORIENTED_EDGE ( 'NONE', *, *, #9047, .T. ) ;
#14117 = AXIS2_PLACEMENT_3D ( 'NONE', #14711, #2554, #10848 ) ;
#14118 = CARTESIAN_POINT ( 'NONE',  ( 10.00000000000000000, -84.79630770241089976, 6.691460262315113816 ) ) ;
#14119 = ORIENTED_EDGE ( 'NONE', *, *, #13213, .F. ) ;
#14120 = EDGE_LOOP ( 'NONE', ( #5562, #18620, #223, #20351 ) ) ;
#14121 = ORIENTED_EDGE ( 'NONE', *, *, #17571, .T. ) ;
#14122 = DIRECTION ( 'NONE',  ( -1.000000000000000000, 0.000000000000000000, 0.000000000000000000 ) ) ;
#14123 = EDGE_LOOP ( 'NONE', ( #8556, #7866, #3058, #2206 ) ) ;
#14124 = DIRECTION ( 'NONE',  ( -1.000000000000000000, 0.000000000000000000, -0.000000000000000000 ) ) ;
#14125 = CARTESIAN_POINT ( 'NONE',  ( 10.00000000000000000, -27.48365448817207479, 0.9185515634840949462 ) ) ;
#14126 = DIRECTION ( 'NONE',  ( 0.000000000000000000, 0.000000000000000000, 1.000000000000000000 ) ) ;
#14127 = DIRECTION ( 'NONE',  ( 0.000000000000000000, 0.000000000000000000, -1.000000000000000000 ) ) ;
#14128 = DIRECTION ( 'NONE',  ( -1.000000000000000000, -0.000000000000000000, -0.000000000000000000 ) ) ;
#14129 = CARTESIAN_POINT ( 'NONE',  ( 10.00000000000000000, 0.000000000000000000, 0.000000000000000000 ) ) ;
#14130 = CARTESIAN_POINT ( 'NONE',  ( 10.00000000000000000, 0.000000000000000000, 0.000000000000000000 ) ) ;
#14131 = CIRCLE ( 'NONE', #15901, 88.00000000000000000 ) ;
#14132 = DIRECTION ( 'NONE',  ( 1.000000000000000000, -0.000000000000000000, -0.000000000000000000 ) ) ;
#14133 = DIRECTION ( 'NONE',  ( -1.000000000000000000, 0.000000000000000000, 0.000000000000000000 ) ) ;
#14134 = ADVANCED_FACE ( 'NONE', ( #10021 ), #21096, .T. ) ;
#14135 = EDGE_LOOP ( 'NONE', ( #13871, #14121, #1325, #3814 ) ) ;
#14136 = CARTESIAN_POINT ( 'NONE',  ( 10.00000000000000000, 0.000000000000000000, 0.000000000000000000 ) ) ;
#14137 = ORIENTED_EDGE ( 'NONE', *, *, #20947, .T. ) ;
#14138 = VERTEX_POINT ( 'NONE', #8377 ) ;
#14139 = ORIENTED_EDGE ( 'NONE', *, *, #8509, .T. ) ;
#14140 = VERTEX_POINT ( 'NONE', #20427 ) ;
#14141 = ORIENTED_EDGE ( 'NONE', *, *, #3966, .T. ) ;
#14142 = ORIENTED_EDGE ( 'NONE', *, *, #12021, .F. ) ;
#14143 = CARTESIAN_POINT ( 'NONE',  ( 1.129531546211678616, 0.000000000000000000, 0.000000000000000000 ) ) ;
#14144 = ORIENTED_EDGE ( 'NONE', *, *, #16809, .F. ) ;
#14145 = DIRECTION ( 'NONE',  ( 0.000000000000000000, -0.9993908270190960952, 0.03489949670249099800 ) ) ;
#14146 = DIRECTION ( 'NONE',  ( -1.000000000000000000, 0.000000000000000000, 0.000000000000000000 ) ) ;
#14147 = DIRECTION ( 'NONE',  ( 0.000000000000000000, 0.000000000000000000, -1.000000000000000000 ) ) ;
#14148 = CARTESIAN_POINT ( 'NONE',  ( 10.00000000000000000, 21.98203405400978383, -17.64965094506522192 ) ) ;
#14149 = DIRECTION ( 'NONE',  ( -1.000000000000000000, -0.000000000000000000, -0.000000000000000000 ) ) ;
#14150 = DIRECTION ( 'NONE',  ( 0.000000000000000000, 0.8987940462991681478, -0.4383711467890751279 ) ) ;
#14151 = CARTESIAN_POINT ( 'NONE',  ( 0.000000000000000000, 85.05652083079336023, -0.7600687895862878740 ) ) ;
#14152 = CARTESIAN_POINT ( 'NONE',  ( 10.00000000000000000, 87.92084725184948013, 3.731570516143270400 ) ) ;
#14153 = EDGE_CURVE ( 'NONE', #6657, #7767, #12254, .T. ) ;
#14154 = ORIENTED_EDGE ( 'NONE', *, *, #12863, .T. ) ;
#14155 = CARTESIAN_POINT ( 'NONE',  ( 10.00000000000000000, 22.77465461094674026, 15.41136296218094159 ) ) ;
#14156 = EDGE_CURVE ( 'NONE', #17938, #15909, #1522, .T. ) ;
#14157 = DIRECTION ( 'NONE',  ( -1.000000000000000000, 0.000000000000000000, -0.000000000000000000 ) ) ;
#14158 = CARTESIAN_POINT ( 'NONE',  ( 5.000000000000002665, -29.47587714451095309, 82.91666097089111531 ) ) ;
#14159 = ORIENTED_EDGE ( 'NONE', *, *, #11220, .F. ) ;
#14160 = DIRECTION ( 'NONE',  ( 0.000000000000000000, 0.000000000000000000, 1.000000000000000000 ) ) ;
#14161 = ORIENTED_EDGE ( 'NONE', *, *, #2716, .F. ) ;
#14162 = FILL_AREA_STYLE ('',( #12503 ) ) ;
#14163 = ADVANCED_FACE ( 'NONE', ( #1145 ), #7668, .F. ) ;
#14164 = DIRECTION ( 'NONE',  ( 1.000000000000000000, 0.000000000000000000, 0.000000000000000000 ) ) ;
#14165 = ORIENTED_EDGE ( 'NONE', *, *, #9493, .F. ) ;
#14166 = ORIENTED_EDGE ( 'NONE', *, *, #1322, .F. ) ;
#14167 = CYLINDRICAL_SURFACE ( 'NONE', #6525, 100.0000000000000284 ) ;
#14168 = CARTESIAN_POINT ( 'NONE',  ( 10.00000000000000000, 51.10509369859540385, -77.10190917907144126 ) ) ;
#14169 = SHAPE_REPRESENTATION ( 'planet connector', ( #15567 ), #16627 ) ;
#14170 = LINE ( 'NONE', #12511, #14988 ) ;
#14171 = DIRECTION ( 'NONE',  ( 0.000000000000000000, -1.603655480014115143E-14, -1.000000000000000000 ) ) ;
#14172 = DIRECTION ( 'NONE',  ( -1.000000000000000000, 0.000000000000000000, 0.000000000000000000 ) ) ;
#14173 = DIRECTION ( 'NONE',  ( 1.000000000000000000, 0.000000000000000000, 0.000000000000000000 ) ) ;
#14174 = AXIS2_PLACEMENT_3D ( 'NONE', #8586, #17209, #10343 ) ;
#14175 = CARTESIAN_POINT ( 'NONE',  ( 0.000000000000000000, 31.15801000616834315, 79.14775961996400611 ) ) ;
#14176 = DIRECTION ( 'NONE',  ( 0.000000000000000000, 0.000000000000000000, 1.000000000000000000 ) ) ;
#14177 = CYLINDRICAL_SURFACE ( 'NONE', #3807, 92.50100000000000477 ) ;
#14178 = EDGE_CURVE ( 'NONE', #15448, #9457, #11558, .T. ) ;
#14179 = EDGE_CURVE ( 'NONE', #9611, #16266, #14022, .T. ) ;
#14180 = EDGE_CURVE ( 'NONE', #15608, #1543, #21156, .T. ) ;
#14181 = ORIENTED_EDGE ( 'NONE', *, *, #2874, .F. ) ;
#14182 = DIRECTION ( 'NONE',  ( 1.000000000000000000, 0.000000000000000000, 0.000000000000000000 ) ) ;
#14183 = ADVANCED_FACE ( 'NONE', ( #2362 ), #21366, .F. ) ;
#14184 = VERTEX_POINT ( 'NONE', #5906 ) ;
#14185 = DIRECTION ( 'NONE',  ( 1.000000000000000000, 0.000000000000000000, 0.000000000000000000 ) ) ;
#14186 = ORIENTED_EDGE ( 'NONE', *, *, #9277, .T. ) ;
#14187 = DIRECTION ( 'NONE',  ( -1.000000000000000000, -0.000000000000000000, 0.000000000000000000 ) ) ;
#14188 = AXIS2_PLACEMENT_3D ( 'NONE', #17586, #14146, #6991 ) ;
#14189 = DIRECTION ( 'NONE',  ( 0.000000000000000000, 0.000000000000000000, 1.000000000000000000 ) ) ;
#14190 = EDGE_LOOP ( 'NONE', ( #642, #15587, #6876, #20029 ) ) ;
#14191 = ADVANCED_FACE ( 'NONE', ( #807 ), #19600, .F. ) ;
#14192 = VERTEX_POINT ( 'NONE', #16175 ) ;
#14193 = AXIS2_PLACEMENT_3D ( 'NONE', #11607, #8401, #11932 ) ;
#14194 = ORIENTED_EDGE ( 'NONE', *, *, #595, .T. ) ;
#14195 = ORIENTED_EDGE ( 'NONE', *, *, #5710, .F. ) ;
#14196 = DIRECTION ( 'NONE',  ( 1.000000000000000000, 0.000000000000000000, 0.000000000000000000 ) ) ;
#14197 = CARTESIAN_POINT ( 'NONE',  ( 5.000000000000000000, 8.660254037844385522, 9.999999999999998224 ) ) ;
#14198 = TOROIDAL_SURFACE ( 'NONE', #20564, 105.0992000000000104, 0.2041999999999998816 ) ;
#14199 = ORIENTED_EDGE ( 'NONE', *, *, #2710, .F. ) ;
#14200 = EDGE_CURVE ( 'NONE', #7490, #9061, #17625, .T. ) ;
#14201 = CARTESIAN_POINT ( 'NONE',  ( 0.000000000000000000, 40.72878876293257377, -78.00747250042405767 ) ) ;
#14202 = CARTESIAN_POINT ( 'NONE',  ( 10.00000000000000000, -81.97107881582211064, 22.71412948308539370 ) ) ;
#14203 = CARTESIAN_POINT ( 'NONE',  ( 0.000000000000000000, 57.06999622551897033, -66.98518889142023625 ) ) ;
#14204 = CARTESIAN_POINT ( 'NONE',  ( 10.00000000000000000, 92.32475887865426500, 5.707354816230855832 ) ) ;
#14205 = EDGE_CURVE ( 'NONE', #12588, #6398, #16506, .T. ) ;
#14206 = DIRECTION ( 'NONE',  ( 0.000000000000000000, 0.000000000000000000, 1.000000000000000000 ) ) ;
#14207 = ORIENTED_EDGE ( 'NONE', *, *, #11784, .T. ) ;
#14208 = CARTESIAN_POINT ( 'NONE',  ( 0.000000000000000000, 24.89070495400845573, -84.40647372620476574 ) ) ;
#14209 = AXIS2_PLACEMENT_3D ( 'NONE', #13367, #5086, #20120 ) ;
#14210 = EDGE_CURVE ( 'NONE', #2159, #13683, #10978, .T. ) ;
#14211 = CARTESIAN_POINT ( 'NONE',  ( 0.000000000000000000, -86.54587337002888603, 15.93147207946976707 ) ) ;
#14212 = AXIS2_PLACEMENT_3D ( 'NONE', #4124, #20489, #12190 ) ;
#14213 = CARTESIAN_POINT ( 'NONE',  ( 10.00000000000000000, 0.000000000000000000, 0.000000000000000000 ) ) ;
#14214 = VERTEX_POINT ( 'NONE', #2577 ) ;
#14216 = AXIS2_PLACEMENT_3D ( 'NONE', #5765, #2540, #17481 ) ;
#14215 = DIRECTION ( 'NONE',  ( 1.000000000000000000, 0.000000000000000000, 0.000000000000000000 ) ) ;
#14217 = ORIENTED_EDGE ( 'NONE', *, *, #8275, .T. ) ;
#14218 = CYLINDRICAL_SURFACE ( 'NONE', #15473, 32.00000000000000000 ) ;
#14219 = EDGE_LOOP ( 'NONE', ( #16459, #9082, #17551, #21430 ) ) ;
#14220 = VECTOR ( 'NONE', #21198, 1000.000000000000000 ) ;
#14221 = ORIENTED_EDGE ( 'NONE', *, *, #5813, .T. ) ;
#14222 = ORIENTED_EDGE ( 'NONE', *, *, #19727, .T. ) ;
#14223 = DIRECTION ( 'NONE',  ( 0.000000000000000000, 0.000000000000000000, 1.000000000000000000 ) ) ;
#14224 = EDGE_CURVE ( 'NONE', #14686, #6084, #2042, .T. ) ;
#14225 = ORIENTED_EDGE ( 'NONE', *, *, #9578, .F. ) ;
#14226 = DIRECTION ( 'NONE',  ( 0.000000000000000000, 0.000000000000000000, -1.000000000000000000 ) ) ;
#14227 = AXIS2_PLACEMENT_3D ( 'NONE', #5854, #865, #21506 ) ;
#14228 = DIRECTION ( 'NONE',  ( 0.000000000000000000, 0.6427876096865353661, 0.7660444431189814551 ) ) ;
#14229 = LINE ( 'NONE', #15993, #6120 ) ;
#14230 = ADVANCED_FACE ( 'NONE', ( #18869 ), #3726, .T. ) ;
#14231 = DIRECTION ( 'NONE',  ( -1.000000000000000000, 0.000000000000000000, 0.000000000000000000 ) ) ;
#14232 = CIRCLE ( 'NONE', #2244, 92.50100000000000477 ) ;
#14233 = EDGE_CURVE ( 'NONE', #4066, #18821, #16056, .T. ) ;
#14234 = DIRECTION ( 'NONE',  ( 0.000000000000000000, 0.000000000000000000, 1.000000000000000000 ) ) ;
#14235 = CARTESIAN_POINT ( 'NONE',  ( 8.000000000000007105, 0.000000000000000000, 0.000000000000000000 ) ) ;
#14236 = DIRECTION ( 'NONE',  ( 0.000000000000000000, 0.000000000000000000, -1.000000000000000000 ) ) ;
#14237 = LINE ( 'NONE', #16000, #17199 ) ;
#14238 = DIRECTION ( 'NONE',  ( 0.000000000000000000, 0.9702957262759955848, 0.2419218955996714493 ) ) ;
#14239 = VECTOR ( 'NONE', #2717, 1000.000000000000000 ) ;
#14240 = DIRECTION ( 'NONE',  ( -1.000000000000000000, -0.000000000000000000, 0.000000000000000000 ) ) ;
#14241 = AXIS2_PLACEMENT_3D ( 'NONE', #5442, #13495, #10078 ) ;
#14242 = EDGE_LOOP ( 'NONE', ( #19117, #5431, #11831, #4803 ) ) ;
#14243 = EDGE_LOOP ( 'NONE', ( #9221, #3826, #1273, #14001 ) ) ;
#14244 = AXIS2_PLACEMENT_3D ( 'NONE', #3041, #11104, #9543 ) ;
#14245 = ORIENTED_EDGE ( 'NONE', *, *, #18493, .T. ) ;
#14246 = VERTEX_POINT ( 'NONE', #9103 ) ;
#14247 = ORIENTED_EDGE ( 'NONE', *, *, #3392, .F. ) ;
#14248 = DIRECTION ( 'NONE',  ( -1.000000000000000000, -0.000000000000000000, -0.000000000000000000 ) ) ;
#14249 = CIRCLE ( 'NONE', #1560, 10.49999999999999822 ) ;
#14250 = EDGE_LOOP ( 'NONE', ( #9450, #19744 ) ) ;
#14251 = DIRECTION ( 'NONE',  ( 0.000000000000000000, 0.000000000000000000, 1.000000000000000000 ) ) ;
#14252 = DIRECTION ( 'NONE',  ( 0.000000000000000000, 0.9848077530122084644, -0.1736481776669273336 ) ) ;
#14253 = VECTOR ( 'NONE', #15431, 1000.000000000000000 ) ;
#14254 = DIRECTION ( 'NONE',  ( -1.000000000000000000, 0.000000000000000000, -0.000000000000000000 ) ) ;
#14255 = CARTESIAN_POINT ( 'NONE',  ( -10.00000000000000000, 0.000000000000000000, 0.000000000000000000 ) ) ;
#14256 = CIRCLE ( 'NONE', #10741, 88.00000000000000000 ) ;
#14257 = DIRECTION ( 'NONE',  ( 0.000000000000000000, -0.5299192642332118952, 0.8480480961564216269 ) ) ;
#14258 = CARTESIAN_POINT ( 'NONE',  ( 0.000000000000000000, 26.69209308833517014, -6.612652082459055336 ) ) ;
#14259 = DIRECTION ( 'NONE',  ( -1.000000000000000000, -0.000000000000000000, -0.000000000000000000 ) ) ;
#14260 = ORIENTED_EDGE ( 'NONE', *, *, #19059, .F. ) ;
#14261 = CARTESIAN_POINT ( 'NONE',  ( 5.000000000000000000, 76.53853822673980289, 43.42639941457142072 ) ) ;
#14262 = AXIS2_PLACEMENT_3D ( 'NONE', #918, #14400, #11082 ) ;
#14263 = AXIS2_PLACEMENT_3D ( 'NONE', #18983, #319, #522 ) ;
#14264 = DIRECTION ( 'NONE',  ( 0.000000000000000000, 0.000000000000000000, 1.000000000000000000 ) ) ;
#14265 = VECTOR ( 'NONE', #5788, 1000.000000000000000 ) ;
#14266 = FACE_OUTER_BOUND ( 'NONE', #19396, .T. ) ;
#14267 = ORIENTED_EDGE ( 'NONE', *, *, #17166, .T. ) ;
#14268 = FACE_OUTER_BOUND ( 'NONE', #4654, .T. ) ;
#14269 = ORIENTED_EDGE ( 'NONE', *, *, #2018, .T. ) ;
#14270 = AXIS2_PLACEMENT_3D ( 'NONE', #16701, #11521, #9853 ) ;
#14271 = DIRECTION ( 'NONE',  ( -0.03050010045823824817, -4.439075233459077528E-17, 0.9995347637136176022 ) ) ;
#14272 = CARTESIAN_POINT ( 'NONE',  ( 10.00000000000000000, 35.34277389771534672, 85.48288328206398035 ) ) ;
#14273 = ORIENTED_EDGE ( 'NONE', *, *, #15577, .F. ) ;
#14274 = ADVANCED_FACE ( 'NONE', ( #6027 ), #16278, .F. ) ;
#14275 = ORIENTED_EDGE ( 'NONE', *, *, #20748, .T. ) ;
#14276 = LINE ( 'NONE', #12302, #13201 ) ;
#14277 = CYLINDRICAL_SURFACE ( 'NONE', #9138, 88.00000000000000000 ) ;
#14278 = CIRCLE ( 'NONE', #2993, 44.99999999999999289 ) ;
#14279 = LINE ( 'NONE', #9298, #10391 ) ;
#14280 = DIRECTION ( 'NONE',  ( 0.000000000000000000, 0.000000000000000000, 1.000000000000000000 ) ) ;
#14281 = CIRCLE ( 'NONE', #8979, 45.00000000000000000 ) ;
#14282 = DIRECTION ( 'NONE',  ( -1.000000000000000000, 0.000000000000000000, 0.000000000000000000 ) ) ;
#14283 = DIRECTION ( 'NONE',  ( 0.000000000000000000, 0.000000000000000000, 1.000000000000000000 ) ) ;
#14284 = ADVANCED_FACE ( 'NONE', ( #2477 ), #14177, .F. ) ;
#14285 = AXIS2_PLACEMENT_3D ( 'NONE', #20521, #15545, #2170 ) ;
#14286 = DIRECTION ( 'NONE',  ( 0.000000000000000000, 0.000000000000000000, -1.000000000000000000 ) ) ;
#14287 = LINE ( 'NONE', #19599, #5215 ) ;
#14289 = AXIS2_PLACEMENT_3D ( 'NONE', #361, #3989, #5877 ) ;
#14288 = DIRECTION ( 'NONE',  ( 0.000000000000000000, 0.000000000000000000, 1.000000000000000000 ) ) ;
#14290 = EDGE_LOOP ( 'NONE', ( #7187, #594, #13107, #18706 ) ) ;
#14291 = CIRCLE ( 'NONE', #6561, 92.50100000000000477 ) ;
#14292 = DIRECTION ( 'NONE',  ( -1.000000000000000000, 0.000000000000000000, 0.000000000000000000 ) ) ;
#14293 = EDGE_LOOP ( 'NONE', ( #8847, #2952, #19019, #14721 ) ) ;
#14294 = CIRCLE ( 'NONE', #19952, 44.99999999999998579 ) ;
#14295 = DIRECTION ( 'NONE',  ( 0.000000000000000000, 0.000000000000000000, -1.000000000000000000 ) ) ;
#14296 = ORIENTED_EDGE ( 'NONE', *, *, #16648, .F. ) ;
#14297 = AXIS2_PLACEMENT_3D ( 'NONE', #1370, #19813, #18388 ) ;
#14298 = CIRCLE ( 'NONE', #542, 88.00000000000000000 ) ;
#14299 = DIRECTION ( 'NONE',  ( 0.000000000000000000, -0.6427876096865299260, -0.7660444431189857850 ) ) ;
#14300 = CIRCLE ( 'NONE', #7954, 5.612499999999999822 ) ;
#14301 = EDGE_LOOP ( 'NONE', ( #10610, #7251, #6635, #9129 ) ) ;
#14302 =( NAMED_UNIT ( * ) SI_UNIT ( $, .STERADIAN. ) SOLID_ANGLE_UNIT ( ) );
#14303 = AXIS2_PLACEMENT_3D ( 'NONE', #9382, #17690, #4308 ) ;
#14304 = ORIENTED_EDGE ( 'NONE', *, *, #3499, .T. ) ;
#14305 = ORIENTED_EDGE ( 'NONE', *, *, #14061, .T. ) ;
#14306 = EDGE_CURVE ( 'NONE', #7513, #17141, #15462, .T. ) ;
#14307 = EDGE_CURVE ( 'NONE', #18258, #10685, #295, .T. ) ;
#14308 = EDGE_LOOP ( 'NONE', ( #3279, #7787, #15356, #18885 ) ) ;
#14309 = EDGE_CURVE ( 'NONE', #20292, #17498, #16149, .T. ) ;
#14310 = DIRECTION ( 'NONE',  ( 0.000000000000000000, 0.3420201433256693235, -0.9396926207859080948 ) ) ;
#14311 = DIRECTION ( 'NONE',  ( 0.000000000000000000, -0.6946583704589885944, -0.7193398003386595185 ) ) ;
#14312 = ORIENTED_EDGE ( 'NONE', *, *, #14307, .F. ) ;
#14313 = EDGE_CURVE ( 'NONE', #2674, #11040, #19683, .T. ) ;
#14314 = LINE ( 'NONE', #17532, #4739 ) ;
#14315 = DIRECTION ( 'NONE',  ( 0.000000000000000000, 0.000000000000000000, -1.000000000000000000 ) ) ;
#14316 = CARTESIAN_POINT ( 'NONE',  ( 10.00000000000000000, 0.6021240089805636186, -31.99433460282944708 ) ) ;
#14317 = DIRECTION ( 'NONE',  ( 0.000000000000000000, 0.9271838545667884235, -0.3746065934159096833 ) ) ;
#14318 = AXIS2_PLACEMENT_3D ( 'NONE', #1576, #18165, #8209 ) ;
#14319 = CARTESIAN_POINT ( 'NONE',  ( 2.000000000000000000, 70.00000000000000000, 15.00000000000000000 ) ) ;
#14320 = CIRCLE ( 'NONE', #2661, 44.99999999999999289 ) ;
#14321 = AXIS2_PLACEMENT_3D ( 'NONE', #20069, #64, #6814 ) ;
#14322 = EDGE_LOOP ( 'NONE', ( #150, #5720, #3930, #19776 ) ) ;
#14323 = VECTOR ( 'NONE', #20685, 1000.000000000000000 ) ;
#14324 = DIRECTION ( 'NONE',  ( 0.000000000000000000, 0.000000000000000000, 1.000000000000000000 ) ) ;
#14325 = EDGE_CURVE ( 'NONE', #389, #16104, #2908, .T. ) ;
#14326 = AXIS2_PLACEMENT_3D ( 'NONE', #10948, #21327, #14589 ) ;
#14327 = CARTESIAN_POINT ( 'NONE',  ( 10.00000000000000000, 7.619321854369911051, -26.42235673590683476 ) ) ;
#14328 = EDGE_CURVE ( 'NONE', #8172, #3525, #8404, .T. ) ;
#14329 = DIRECTION ( 'NONE',  ( 0.000000000000000000, 0.000000000000000000, 1.000000000000000000 ) ) ;
#14330 = ORIENTED_EDGE ( 'NONE', *, *, #15106, .F. ) ;
#14331 = DIRECTION ( 'NONE',  ( -1.000000000000000000, 0.000000000000000000, 0.000000000000000000 ) ) ;
#14332 = EDGE_LOOP ( 'NONE', ( #12889, #21718, #21136, #16288 ) ) ;
#14333 = CARTESIAN_POINT ( 'NONE',  ( -5.000000000000000000, 67.00000000000000000, 9.999999999999998224 ) ) ;
#14334 = EDGE_LOOP ( 'NONE', ( #14496, #16838, #19234, #6528 ) ) ;
#14335 = APPLICATION_CONTEXT ( 'automotive_design' ) ;
#14336 = EDGE_LOOP ( 'NONE', ( #14367, #1070, #19116, #20403 ) ) ;
#14337 = CIRCLE ( 'NONE', #5175, 92.50100000000000477 ) ;
#14338 = ORIENTED_EDGE ( 'NONE', *, *, #15652, .F. ) ;
#14339 = DIRECTION ( 'NONE',  ( -1.000000000000000000, 0.000000000000000000, 0.000000000000000000 ) ) ;
#14340 = CIRCLE ( 'NONE', #10461, 100.0000000000000000 ) ;
#14341 = ORIENTED_EDGE ( 'NONE', *, *, #420, .T. ) ;
#14342 = AXIS2_PLACEMENT_3D ( 'NONE', #12229, #20847, #13672 ) ;
#14343 = CARTESIAN_POINT ( 'NONE',  ( 0.000000000000000000, -87.58454185039444440, 8.540961822681374827 ) ) ;
#14344 = EDGE_CURVE ( 'NONE', #19278, #3086, #11738, .T. ) ;
#14345 = FACE_OUTER_BOUND ( 'NONE', #967, .T. ) ;
#14346 = FACE_OUTER_BOUND ( 'NONE', #20384, .T. ) ;
#14347 = CARTESIAN_POINT ( 'NONE',  ( 10.00000000000000000, 0.000000000000000000, 0.000000000000000000 ) ) ;
#14348 = DIRECTION ( 'NONE',  ( -1.000000000000000000, 0.000000000000000000, 0.000000000000000000 ) ) ;
#14349 = CARTESIAN_POINT ( 'NONE',  ( 10.00000000000000000, -83.35585896458606214, -16.94078559808036033 ) ) ;
#14350 = CARTESIAN_POINT ( 'NONE',  ( -8.000000000000007105, 1.409568465818603827E-14, 115.1000000000000227 ) ) ;
#14351 = DIRECTION ( 'NONE',  ( -1.000000000000000000, -0.000000000000000000, 0.000000000000000000 ) ) ;
#14352 = DIRECTION ( 'NONE',  ( 1.000000000000000000, 0.000000000000000000, 0.000000000000000000 ) ) ;
#14353 = ADVANCED_FACE ( 'NONE', ( #18488 ), #4794, .F. ) ;
#14354 = CIRCLE ( 'NONE', #3769, 27.49900000000000233 ) ;
#14355 = EDGE_CURVE ( 'NONE', #15532, #49, #10080, .T. ) ;
#14356 = DIRECTION ( 'NONE',  ( -1.000000000000000000, 0.000000000000000000, 0.000000000000000000 ) ) ;
#14357 = ORIENTED_EDGE ( 'NONE', *, *, #13274, .T. ) ;
#14358 = ORIENTED_EDGE ( 'NONE', *, *, #1322, .T. ) ;
#14359 = EDGE_CURVE ( 'NONE', #17932, #13478, #14038, .T. ) ;
#14360 = EDGE_CURVE ( 'NONE', #8996, #21383, #21479, .T. ) ;
#14361 = VERTEX_POINT ( 'NONE', #19814 ) ;
#14362 = VERTEX_POINT ( 'NONE', #19709 ) ;
#14363 = VERTEX_POINT ( 'NONE', #6575 ) ;
#14364 = DIRECTION ( 'NONE',  ( 0.000000000000000000, 0.8290375725550428454, -0.5591929034707450175 ) ) ;
#14365 = AXIS2_PLACEMENT_3D ( 'NONE', #4407, #4194, #19536 ) ;
#14366 = ADVANCED_FACE ( 'NONE', ( #4675 ), #8442, .F. ) ;
#14367 = ORIENTED_EDGE ( 'NONE', *, *, #14989, .F. ) ;
#14368 = CARTESIAN_POINT ( 'NONE',  ( 10.00000000000000000, 0.000000000000000000, 0.000000000000000000 ) ) ;
#14369 = AXIS2_PLACEMENT_3D ( 'NONE', #15884, #9556, #11007 ) ;
#14370 = CARTESIAN_POINT ( 'NONE',  ( -8.000000000000007105, 0.000000000000000000, 0.000000000000000000 ) ) ;
#14371 = CYLINDRICAL_SURFACE ( 'NONE', #13845, 11.99999999999999822 ) ;
#14372 = DIRECTION ( 'NONE',  ( 0.000000000000000000, -0.5299192642331944647, -0.8480480961564325071 ) ) ;
#14373 = DIRECTION ( 'NONE',  ( 0.000000000000000000, 0.000000000000000000, 1.000000000000000000 ) ) ;
#14374 = DIRECTION ( 'NONE',  ( -1.000000000000000000, 0.000000000000000000, -0.000000000000000000 ) ) ;
#14375 = DIRECTION ( 'NONE',  ( 0.000000000000000000, -0.4067366430758070361, 0.9135454576425978690 ) ) ;
#14376 = CARTESIAN_POINT ( 'NONE',  ( 10.00000000000000000, -28.15804365424196121, 10.64184787299373269 ) ) ;
#14377 = CYLINDRICAL_SURFACE ( 'NONE', #10177, 11.99999999999999645 ) ;
#14378 = ORIENTED_EDGE ( 'NONE', *, *, #17163, .T. ) ;
#14379 = DIRECTION ( 'NONE',  ( -1.000000000000000000, -0.000000000000000000, -0.000000000000000000 ) ) ;
#14380 = CIRCLE ( 'NONE', #20038, 6.887500000000022382 ) ;
#14381 = AXIS2_PLACEMENT_3D ( 'NONE', #20422, #7144, #5281 ) ;
#14382 = AXIS2_PLACEMENT_3D ( 'NONE', #6785, #18811, #8753 ) ;
#14383 = CARTESIAN_POINT ( 'NONE',  ( 10.00000000000000000, 0.000000000000000000, 0.000000000000000000 ) ) ;
#14384 = CARTESIAN_POINT ( 'NONE',  ( 10.00000000000000000, 1.959304526718168571, -27.42911093658673138 ) ) ;
#14385 = ORIENTED_EDGE ( 'NONE', *, *, #9984, .F. ) ;
#14386 = FACE_OUTER_BOUND ( 'NONE', #19800, .T. ) ;
#14387 = EDGE_LOOP ( 'NONE', ( #3652, #5425, #1484, #15840 ) ) ;
#14388 = ORIENTED_EDGE ( 'NONE', *, *, #20544, .T. ) ;
#14389 = CARTESIAN_POINT ( 'NONE',  ( -6.938893903907228378E-15, 4.261831059646176042E-15, -60.00000000000001421 ) ) ;
#14390 = VECTOR ( 'NONE', #8432, 1000.000000000000000 ) ;
#14391 = CARTESIAN_POINT ( 'NONE',  ( 1.500000000000000000, -4.769696007084728073, 100.0000000000000000 ) ) ;
#14392 = ORIENTED_EDGE ( 'NONE', *, *, #2263, .F. ) ;
#14393 = ORIENTED_EDGE ( 'NONE', *, *, #8288, .T. ) ;
#14394 = CARTESIAN_POINT ( 'NONE',  ( -10.00000000000000000, 0.000000000000000000, 0.000000000000000000 ) ) ;
#14395 = DIRECTION ( 'NONE',  ( -1.000000000000000000, 0.000000000000000000, -0.000000000000000000 ) ) ;
#14396 = CIRCLE ( 'NONE', #4879, 92.50100000000000477 ) ;
#14397 = LINE ( 'NONE', #13166, #13930 ) ;
#14398 = CARTESIAN_POINT ( 'NONE',  ( 9.999999999999994671, 0.000000000000000000, 103.6249999999999716 ) ) ;
#14399 = DIRECTION ( 'NONE',  ( 0.000000000000000000, 0.000000000000000000, 1.000000000000000000 ) ) ;
#14400 = DIRECTION ( 'NONE',  ( 1.000000000000000000, 0.000000000000000000, 0.000000000000000000 ) ) ;
#14401 = CIRCLE ( 'NONE', #7004, 44.99999999999999289 ) ;
#14402 = CARTESIAN_POINT ( 'NONE',  ( 10.00000000000000000, -86.66425444033941972, 32.33793443156368852 ) ) ;
#14403 = CARTESIAN_POINT ( 'NONE',  ( 10.00000000000000000, 9.366510754379572035, -25.85466064925416774 ) ) ;
#14404 = CARTESIAN_POINT ( 'NONE',  ( 10.00000000000000000, 45.60224695560570041, 80.47900393021744492 ) ) ;
#14405 = ORIENTED_EDGE ( 'NONE', *, *, #1236, .T. ) ;
#14406 = DIRECTION ( 'NONE',  ( 0.000000000000000000, 0.8660254037844363761, 0.5000000000000039968 ) ) ;
#14407 = ADVANCED_FACE ( 'NONE', ( #11307 ), #16711, .F. ) ;
#14408 = VERTEX_POINT ( 'NONE', #8324 ) ;
#14409 = CARTESIAN_POINT ( 'NONE',  ( 10.00000000000000000, 43.18649929580192293, 73.28107340219430910 ) ) ;
#14410 = SURFACE_STYLE_USAGE ( .BOTH. , #7675 ) ;
#14411 = AXIS2_PLACEMENT_3D ( 'NONE', #11176, #2889, #5190 ) ;
#14412 = CIRCLE ( 'NONE', #13712, 32.00000000000000000 ) ;
#14413 = AXIS2_PLACEMENT_3D ( 'NONE', #12393, #4004, #4445 ) ;
#14414 = CARTESIAN_POINT ( 'NONE',  ( 10.00000000000000000, 0.000000000000000000, 0.000000000000000000 ) ) ;
#14415 = CIRCLE ( 'NONE', #11602, 101.1000000000000512 ) ;
#14416 = CIRCLE ( 'NONE', #651, 92.50099999999999056 ) ;
#14417 = ORIENTED_EDGE ( 'NONE', *, *, #20268, .F. ) ;
#14418 = PRODUCT_RELATED_PRODUCT_CATEGORY ( 'part', '', ( #13018 ) ) ;
#14419 = FILL_AREA_STYLE_COLOUR ( '', #2504 ) ;
#14420 = EDGE_LOOP ( 'NONE', ( #14782, #2479, #20587, #4277 ) ) ;
#14421 = ORIENTED_EDGE ( 'NONE', *, *, #9403, .T. ) ;
#14422 = VERTEX_POINT ( 'NONE', #1468 ) ;
#14423 = CARTESIAN_POINT ( 'NONE',  ( 10.00000000000000000, -23.10190250628773967, -89.56973317806621537 ) ) ;
#14424 = CARTESIAN_POINT ( 'NONE',  ( 0.000000000000000000, 0.000000000000000000, 0.000000000000000000 ) ) ;
#14425 = ORIENTED_EDGE ( 'NONE', *, *, #17266, .T. ) ;
#14426 = DIRECTION ( 'NONE',  ( -1.000000000000000000, -0.000000000000000000, 0.000000000000000000 ) ) ;
#14427 = CARTESIAN_POINT ( 'NONE',  ( 0.000000000000000000, -51.76708072107932423, 67.49339815138475274 ) ) ;
#14428 = LINE ( 'NONE', #12760, #18551 ) ;
#14429 = CIRCLE ( 'NONE', #17260, 32.00000000000000000 ) ;
#14430 = LINE ( 'NONE', #21176, #130 ) ;
#14431 = CARTESIAN_POINT ( 'NONE',  ( 0.000000000000000000, 65.83713140174729972, 58.39068529131218099 ) ) ;
#14432 = CIRCLE ( 'NONE', #7735, 5.612499999999999822 ) ;
#14433 = COLOUR_RGB ( '', 0.08235294, 0.09019608, 0.10196078) ;
#14434 = ORIENTED_EDGE ( 'NONE', *, *, #12851, .F. ) ;
#14435 = AXIS2_PLACEMENT_3D ( 'NONE', #18579, #3755, #20555 ) ;
#14436 = CARTESIAN_POINT ( 'NONE',  ( 10.00000000000000000, 0.000000000000000000, 0.000000000000000000 ) ) ;
#14437 = CYLINDRICAL_SURFACE ( 'NONE', #19592, 27.49900000000000233 ) ;
#14438 = ADVANCED_FACE ( 'NONE', ( #13289 ), #15056, .F. ) ;
#14439 = DIRECTION ( 'NONE',  ( 1.000000000000000000, 0.000000000000000000, 0.000000000000000000 ) ) ;
#14440 = VERTEX_POINT ( 'NONE', #14840 ) ;
#14441 = CYLINDRICAL_SURFACE ( 'NONE', #3493, 92.50100000000000477 ) ;
#14442 = ORIENTED_EDGE ( 'NONE', *, *, #13381, .T. ) ;
#14443 = CARTESIAN_POINT ( 'NONE',  ( -90.00000000000000000, 0.000000000000000000, -5.612499999999999822 ) ) ;
#14444 = ORIENTED_EDGE ( 'NONE', *, *, #17340, .F. ) ;
#14445 = PLANE ( 'NONE',  #9180 ) ;
#14446 = CIRCLE ( 'NONE', #17276, 44.99999999999998579 ) ;
#14447 = VERTEX_POINT ( 'NONE', #4904 ) ;
#14448 = AXIS2_PLACEMENT_3D ( 'NONE', #21806, #9641, #15063 ) ;
#14449 = ORIENTED_EDGE ( 'NONE', *, *, #6004, .F. ) ;
#14450 = AXIS2_PLACEMENT_3D ( 'NONE', #2585, #4254, #19392 ) ;
#14451 = CYLINDRICAL_SURFACE ( 'NONE', #16791, 11.99999999999999822 ) ;
#14452 = CIRCLE ( 'NONE', #11637, 44.99999999999999289 ) ;
#14453 = VERTEX_POINT ( 'NONE', #13172 ) ;
#14454 = EDGE_CURVE ( 'NONE', #16474, #1041, #21582, .T. ) ;
#14455 = DIRECTION ( 'NONE',  ( 0.000000000000000000, -0.8660254037844328234, -0.5000000000000101030 ) ) ;
#14456 = DIRECTION ( 'NONE',  ( -1.000000000000000000, 0.000000000000000000, 0.000000000000000000 ) ) ;
#14457 = DIRECTION ( 'NONE',  ( -1.000000000000000000, 0.000000000000000000, -0.000000000000000000 ) ) ;
#14458 = LINE ( 'NONE', #17669, #14220 ) ;
#14459 = EDGE_CURVE ( 'NONE', #1120, #6202, #17580, .T. ) ;
#14460 = DIRECTION ( 'NONE',  ( -1.000000000000000000, -0.000000000000000000, 0.000000000000000000 ) ) ;
#14461 = DIRECTION ( 'NONE',  ( 0.000000000000000000, -0.9848077530122096857, 0.1736481776669207000 ) ) ;
#14462 = DIRECTION ( 'NONE',  ( 0.000000000000000000, 0.000000000000000000, 1.000000000000000000 ) ) ;
#14463 = CYLINDRICAL_SURFACE ( 'NONE', #333, 92.50100000000000477 ) ;
#14464 = EDGE_CURVE ( 'NONE', #10717, #16982, #11645, .T. ) ;
#14465 = EDGE_CURVE ( 'NONE', #535, #20663, #4524, .T. ) ;
#14466 = EDGE_CURVE ( 'NONE', #4022, #6777, #2059, .T. ) ;
#14467 = AXIS2_PLACEMENT_3D ( 'NONE', #3350, #13509, #21693 ) ;
#14468 = CARTESIAN_POINT ( 'NONE',  ( 10.00000000000000000, 74.74361964203228581, -40.60271866773572214 ) ) ;
#14469 = APPLICATION_CONTEXT ( 'automotive_design' ) ;
#14470 = EDGE_LOOP ( 'NONE', ( #11646, #16188, #17651, #3176 ) ) ;
#14471 = EDGE_CURVE ( 'NONE', #11540, #17704, #14401, .T. ) ;
#14472 = ORIENTED_EDGE ( 'NONE', *, *, #9895, .F. ) ;
#14473 = VERTEX_POINT ( 'NONE', #13834 ) ;
#14474 = ORIENTED_EDGE ( 'NONE', *, *, #14843, .F. ) ;
#14475 = ORIENTED_EDGE ( 'NONE', *, *, #9726, .F. ) ;
#14476 = EDGE_CURVE ( 'NONE', #2910, #10178, #13617, .T. ) ;
#14477 = DIRECTION ( 'NONE',  ( -1.000000000000000000, -0.000000000000000000, -0.000000000000000000 ) ) ;
#14478 = ORIENTED_EDGE ( 'NONE', *, *, #11225, .F. ) ;
#14479 = CARTESIAN_POINT ( 'NONE',  ( 10.00000000000000000, 0.000000000000000000, 0.000000000000000000 ) ) ;
#14480 = AXIS2_PLACEMENT_3D ( 'NONE', #1559, #3325, #4770 ) ;
#14481 = EDGE_CURVE ( 'NONE', #6576, #10476, #4882, .T. ) ;
#14482 = FACE_OUTER_BOUND ( 'NONE', #2950, .T. ) ;
#14483 = DIRECTION ( 'NONE',  ( 0.000000000000000000, -9.714451465470122884E-15, -1.000000000000000000 ) ) ;
#14484 = EDGE_CURVE ( 'NONE', #11183, #4150, #4867, .T. ) ;
#14485 = FACE_OUTER_BOUND ( 'NONE', #20025, .T. ) ;
#14486 = CARTESIAN_POINT ( 'NONE',  ( 10.00000000000000000, -41.21966518005896774, -82.80926399530329718 ) ) ;
#14487 = DIRECTION ( 'NONE',  ( -1.000000000000000000, 0.000000000000000000, 0.000000000000000000 ) ) ;
#14488 = EDGE_CURVE ( 'NONE', #8283, #18366, #14754, .T. ) ;
#14489 = DIRECTION ( 'NONE',  ( 0.000000000000000000, 0.3420201433256631063, 0.9396926207859105373 ) ) ;
#14490 = CYLINDRICAL_SURFACE ( 'NONE', #13992, 32.00000000000000000 ) ;
#14491 = LINE ( 'NONE', #17804, #2416 ) ;
#14492 = ORIENTED_EDGE ( 'NONE', *, *, #939, .F. ) ;
#14493 = CARTESIAN_POINT ( 'NONE',  ( 10.00000000000000000, 78.01214607583752070, 33.90124636420136994 ) ) ;
#14494 = ADVANCED_FACE ( 'NONE', ( #15376 ), #252, .F. ) ;
#14495 = VECTOR ( 'NONE', #21728, 1000.000000000000000 ) ;
#14496 = ORIENTED_EDGE ( 'NONE', *, *, #12850, .F. ) ;
#14497 = DIRECTION ( 'NONE',  ( 0.000000000000000000, -0.4694715627858797591, -0.8829475928589327616 ) ) ;
#14498 = CYLINDRICAL_SURFACE ( 'NONE', #3191, 126.5000000000000000 ) ;
#14499 = ORIENTED_EDGE ( 'NONE', *, *, #13544, .F. ) ;
#14500 = LINE ( 'NONE', #16036, #897 ) ;
#14501 = ORIENTED_EDGE ( 'NONE', *, *, #21199, .T. ) ;
#14502 = ORIENTED_EDGE ( 'NONE', *, *, #3110, .F. ) ;
#14503 = CARTESIAN_POINT ( 'NONE',  ( 0.000000000000000000, 17.70753755129037188, 21.03896658273978559 ) ) ;
#14504 = ORIENTED_EDGE ( 'NONE', *, *, #19154, .F. ) ;
#14505 = ORIENTED_EDGE ( 'NONE', *, *, #20152, .F. ) ;
#14506 = CARTESIAN_POINT ( 'NONE',  ( 0.000000000000000000, 0.000000000000000000, -3.000000000000000000 ) ) ;
#14507 = EDGE_CURVE ( 'NONE', #11658, #8121, #17223, .T. ) ;
#14508 = CARTESIAN_POINT ( 'NONE',  ( 5.000000000000002665, -17.64925110578410639, -86.21197095186363413 ) ) ;
#14509 = CARTESIAN_POINT ( 'NONE',  ( 7.440711023145602176, 0.000000000000000000, -115.1000000000000227 ) ) ;
#14510 = LINE ( 'NONE', #16047, #6299 ) ;
#14511 = CARTESIAN_POINT ( 'NONE',  ( 10.00000000000000000, -19.29292659243987629, -25.53004080487781735 ) ) ;
#14512 = PRESENTATION_LAYER_ASSIGNMENT (  '', '', ( #11697 ) ) ;
#14513 = CARTESIAN_POINT ( 'NONE',  ( 10.00000000000000000, 0.000000000000000000, 0.000000000000000000 ) ) ;
#14514 = ADVANCED_FACE ( 'NONE', ( #17272 ), #10403, .F. ) ;
#14515 = CARTESIAN_POINT ( 'NONE',  ( 0.000000000000000000, -15.32665449651862843, -91.22241316115434984 ) ) ;
#14516 = CARTESIAN_POINT ( 'NONE',  ( 10.00000000000000000, 0.000000000000000000, 0.000000000000000000 ) ) ;
#14517 = ORIENTED_EDGE ( 'NONE', *, *, #8527, .T. ) ;
#14518 = CARTESIAN_POINT ( 'NONE',  ( 5.000000000000000000, -12.46320060045703038, -29.47318494484041196 ) ) ;
#14519 = VERTEX_POINT ( 'NONE', #3569 ) ;
#14520 = CARTESIAN_POINT ( 'NONE',  ( 0.000000000000000000, 82.02147376274727719, -42.76579056660780509 ) ) ;
#14521 = DIRECTION ( 'NONE',  ( -1.000000000000000000, 0.000000000000000000, 0.000000000000000000 ) ) ;
#14522 =( GEOMETRIC_REPRESENTATION_CONTEXT ( 3 ) GLOBAL_UNCERTAINTY_ASSIGNED_CONTEXT ( ( #4818 ) ) GLOBAL_UNIT_ASSIGNED_CONTEXT ( ( #2589, #4476, #8220 ) ) REPRESENTATION_CONTEXT ( 'NONE', 'WORKASPACE' ) );
#14523 = CARTESIAN_POINT ( 'NONE',  ( 10.00000000000000000, 84.90234713953985590, 5.175025661884123274 ) ) ;
#14524 = ORIENTED_EDGE ( 'NONE', *, *, #1781, .F. ) ;
#14525 =( LENGTH_UNIT ( ) NAMED_UNIT ( * ) SI_UNIT ( .MILLI., .METRE. ) );
#14526 = EDGE_LOOP ( 'NONE', ( #16576, #3919, #16860, #15834 ) ) ;
#14527 = ORIENTED_EDGE ( 'NONE', *, *, #11657, .F. ) ;
#14528 = VERTEX_POINT ( 'NONE', #10297 ) ;
#14529 = DIRECTION ( 'NONE',  ( 0.000000000000000000, 0.5299192642332060110, -0.8480480961564252906 ) ) ;
#14530 = DIRECTION ( 'NONE',  ( -1.000000000000000000, 0.000000000000000000, 0.000000000000000000 ) ) ;
#14531 = EDGE_CURVE ( 'NONE', #18170, #4150, #10159, .T. ) ;
#14532 = ORIENTED_EDGE ( 'NONE', *, *, #19778, .T. ) ;
#14533 = CARTESIAN_POINT ( 'NONE',  ( 0.000000000000000000, 15.00000000000000000, 0.000000000000000000 ) ) ;
#14534 = DIRECTION ( 'NONE',  ( -1.000000000000000000, -0.000000000000000000, -0.000000000000000000 ) ) ;
#14535 = DIRECTION ( 'NONE',  ( -1.000000000000000000, -0.000000000000000000, -0.000000000000000000 ) ) ;
#14536 = DIRECTION ( 'NONE',  ( 1.000000000000000000, 0.000000000000000000, 0.000000000000000000 ) ) ;
#14537 = CARTESIAN_POINT ( 'NONE',  ( 5.000000000000000000, -57.06999622551760609, -66.98518889142141575 ) ) ;
#14538 = PRODUCT_DEFINITION_FORMATION_WITH_SPECIFIED_SOURCE ( 'ANY', '', #13018, .NOT_KNOWN. ) ;
#14539 = ORIENTED_EDGE ( 'NONE', *, *, #3265, .F. ) ;
#14540 = LINE ( 'NONE', #21281, #1848 ) ;
#14541 = AXIS2_PLACEMENT_3D ( 'NONE', #9169, #7634, #14252 ) ;
#14542 = DIRECTION ( 'NONE',  ( 1.000000000000000000, -0.000000000000000000, -0.000000000000000000 ) ) ;
#14543 = ORIENTED_EDGE ( 'NONE', *, *, #675, .F. ) ;
#14544 = DIRECTION ( 'NONE',  ( 0.000000000000000000, 0.8660254037844398178, -0.4999999999999979461 ) ) ;
#14545 = ORIENTED_EDGE ( 'NONE', *, *, #4083, .F. ) ;
#14546 = AXIS2_PLACEMENT_3D ( 'NONE', #5137, #8457, #17063 ) ;
#14547 = DIRECTION ( 'NONE',  ( 1.000000000000000000, 0.000000000000000000, 0.000000000000000000 ) ) ;
#14548 = DIRECTION ( 'NONE',  ( 1.000000000000000000, -0.000000000000000000, -0.000000000000000000 ) ) ;
#14549 = VERTEX_POINT ( 'NONE', #8859 ) ;
#14550 = DIRECTION ( 'NONE',  ( 1.000000000000000000, 0.000000000000000000, 0.000000000000000000 ) ) ;
#14551 = ORIENTED_EDGE ( 'NONE', *, *, #2867, .T. ) ;
#14552 = VERTEX_POINT ( 'NONE', #11855 ) ;
#14553 = DIRECTION ( 'NONE',  ( 0.000000000000000000, -1.000000000000000000, 0.000000000000000000 ) ) ;
#14554 = ORIENTED_EDGE ( 'NONE', *, *, #17717, .T. ) ;
#14555 = FACE_OUTER_BOUND ( 'NONE', #1729, .T. ) ;
#14556 = AXIS2_PLACEMENT_3D ( 'NONE', #10045, #13365, #18245 ) ;
#14557 = CARTESIAN_POINT ( 'NONE',  ( 0.000000000000000000, -73.32282170386882569, 48.65967342042752364 ) ) ;
#14558 = CARTESIAN_POINT ( 'NONE',  ( -1.500000000000000000, -7.000000000000000000, 5.000000000000000000 ) ) ;
#14559 = EDGE_CURVE ( 'NONE', #15964, #13385, #6998, .T. ) ;
#14560 = AXIS2_PLACEMENT_3D ( 'NONE', #16577, #14912, #21762 ) ;
#14561 = CARTESIAN_POINT ( 'NONE',  ( 0.000000000000000000, 0.000000000000000000, 0.000000000000000000 ) ) ;
#14562 = DIRECTION ( 'NONE',  ( -1.000000000000000000, 0.000000000000000000, 0.000000000000000000 ) ) ;
#14563 = EDGE_CURVE ( 'NONE', #21750, #8568, #10504, .T. ) ;
#14564 = DIRECTION ( 'NONE',  ( 0.000000000000000000, -0.6427876096865456912, 0.7660444431189725734 ) ) ;
#14565 = PLANE ( 'NONE',  #16186 ) ;
#14566 = CYLINDRICAL_SURFACE ( 'NONE', #18594, 44.99999999999998579 ) ;
#14567 = ADVANCED_FACE ( 'NONE', ( #17044 ), #1904, .F. ) ;
#14568 = ORIENTED_EDGE ( 'NONE', *, *, #21733, .F. ) ;
#14569 = STYLED_ITEM ( 'NONE', ( #15672 ), #6054 ) ;
#14570 = ORIENTED_EDGE ( 'NONE', *, *, #17576, .F. ) ;
#14571 = EDGE_LOOP ( 'NONE', ( #16730, #17969, #6704, #15415 ) ) ;
#14572 = CIRCLE ( 'NONE', #7880, 123.5000000000000142 ) ;
#14573 = AXIS2_PLACEMENT_3D ( 'NONE', #12901, #7609, #6068 ) ;
#14574 = ORIENTED_EDGE ( 'NONE', *, *, #272, .T. ) ;
#14575 = VECTOR ( 'NONE', #5131, 1000.000000000000000 ) ;
#14576 = ORIENTED_EDGE ( 'NONE', *, *, #3947, .T. ) ;
#14577 = CARTESIAN_POINT ( 'NONE',  ( 10.00000000000000000, 0.000000000000000000, 0.000000000000000000 ) ) ;
#14578 = ADVANCED_FACE ( 'NONE', ( #8640 ), #10623, .T. ) ;
#14579 = ORIENTED_EDGE ( 'NONE', *, *, #8246, .T. ) ;
#14580 = CARTESIAN_POINT ( 'NONE',  ( 10.00000000000000000, 92.22057093985031884, 7.197311757040840696 ) ) ;
#14581 = EDGE_CURVE ( 'NONE', #5619, #6428, #4168, .T. ) ;
#14582 = EDGE_CURVE ( 'NONE', #19694, #20559, #2398, .T. ) ;
#14583 = DIRECTION ( 'NONE',  ( -1.000000000000000000, -0.000000000000000000, -0.000000000000000000 ) ) ;
#14584 = ADVANCED_FACE ( 'NONE', ( #37 ), #3458, .T. ) ;
#14585 = CIRCLE ( 'NONE', #3642, 7.500000000000000000 ) ;
#14586 = FACE_OUTER_BOUND ( 'NONE', #10299, .T. ) ;
#14587 = DIRECTION ( 'NONE',  ( 0.000000000000000000, 0.8987940462991649282, 0.4383711467890815117 ) ) ;
#14588 = DIRECTION ( 'NONE',  ( -1.000000000000000000, -0.000000000000000000, -0.000000000000000000 ) ) ;
#14589 = DIRECTION ( 'NONE',  ( 0.000000000000000000, 0.000000000000000000, 1.000000000000000000 ) ) ;
#14590 = CARTESIAN_POINT ( 'NONE',  ( 10.00000000000000000, 25.48117629651189375, 10.33947075754270095 ) ) ;
#14591 = DIRECTION ( 'NONE',  ( 1.000000000000000000, 0.000000000000000000, 0.000000000000000000 ) ) ;
#14592 = CIRCLE ( 'NONE', #1896, 45.00000000000000000 ) ;
#14593 = ORIENTED_EDGE ( 'NONE', *, *, #1470, .T. ) ;
#14594 = CIRCLE ( 'NONE', #15648, 45.00000000000000000 ) ;
#14595 = FACE_OUTER_BOUND ( 'NONE', #6870, .T. ) ;
#14596 = EDGE_CURVE ( 'NONE', #1794, #16126, #9114, .T. ) ;
#14597 = ORIENTED_EDGE ( 'NONE', *, *, #8112, .F. ) ;
#14598 = FACE_OUTER_BOUND ( 'NONE', #963, .T. ) ;
#14599 = EDGE_CURVE ( 'NONE', #18557, #3682, #10519, .T. ) ;
#14600 = DIRECTION ( 'NONE',  ( 1.000000000000000000, 0.000000000000000000, 0.000000000000000000 ) ) ;
#14601 = AXIS2_PLACEMENT_3D ( 'NONE', #5824, #7583, #10893 ) ;
#14602 = VERTEX_POINT ( 'NONE', #9176 ) ;
#14603 = CARTESIAN_POINT ( 'NONE',  ( 0.000000000000000000, 84.33453774737672859, -11.08490790852044405 ) ) ;
#14604 = ORIENTED_EDGE ( 'NONE', *, *, #9365, .F. ) ;
#14605 = ORIENTED_EDGE ( 'NONE', *, *, #12702, .T. ) ;
#14606 = CARTESIAN_POINT ( 'NONE',  ( 2.140611735271801307E-16, 9.999999999999992895, 4.506460675456329944E-16 ) ) ;
#14607 = VECTOR ( 'NONE', #8895, 1000.000000000000000 ) ;
#14608 = FACE_OUTER_BOUND ( 'NONE', #6274, .T. ) ;
#14609 = VERTEX_POINT ( 'NONE', #9071 ) ;
#14610 = ORIENTED_EDGE ( 'NONE', *, *, #10161, .F. ) ;
#14611 = DIRECTION ( 'NONE',  ( -1.000000000000000000, -0.000000000000000000, 0.000000000000000000 ) ) ;
#14612 = LINE ( 'NONE', #21355, #19753 ) ;
#14613 = EDGE_CURVE ( 'NONE', #9954, #1233, #14491, .T. ) ;
#14614 = CARTESIAN_POINT ( 'NONE',  ( 0.000000000000000000, -61.33825423015638734, -69.23910433416007493 ) ) ;
#14615 = PLANE ( 'NONE',  #20238 ) ;
#14616 = DIRECTION ( 'NONE',  ( 0.000000000000000000, 0.9271838545667857590, 0.3746065934159159561 ) ) ;
#14617 = LINE ( 'NONE', #4459, #17469 ) ;
#14618 = CARTESIAN_POINT ( 'NONE',  ( 10.00000000000000000, 81.97107881582195432, 22.71412948308594437 ) ) ;
#14619 = CARTESIAN_POINT ( 'NONE',  ( 0.000000000000000000, 5.000000000000000000, 3.000000000000002665 ) ) ;
#14620 = DIRECTION ( 'NONE',  ( -1.000000000000000000, -0.000000000000000000, -0.000000000000000000 ) ) ;
#14621 = AXIS2_PLACEMENT_3D ( 'NONE', #8670, #18839, #8462 ) ;
#14622 = ORIENTED_EDGE ( 'NONE', *, *, #118, .T. ) ;
#14623 = DIRECTION ( 'NONE',  ( -1.000000000000000000, 0.000000000000000000, 0.000000000000000000 ) ) ;
#14624 = EDGE_CURVE ( 'NONE', #20437, #21516, #14774, .T. ) ;
#14625 = CIRCLE ( 'NONE', #172, 5.612499999999999822 ) ;
#14626 = ORIENTED_EDGE ( 'NONE', *, *, #9969, .T. ) ;
#14627 = EDGE_CURVE ( 'NONE', #8596, #13627, #6318, .T. ) ;
#14628 = CARTESIAN_POINT ( 'NONE',  ( -10.00000000000002309, 0.000000000000000000, 0.000000000000000000 ) ) ;
#14629 = CARTESIAN_POINT ( 'NONE',  ( 10.00000000000000000, 68.36541360927260769, -50.60987712331631627 ) ) ;
#14630 = EDGE_CURVE ( 'NONE', #428, #16396, #11603, .T. ) ;
#14631 = CYLINDRICAL_SURFACE ( 'NONE', #19737, 11.99999999999999822 ) ;
#14632 = ORIENTED_EDGE ( 'NONE', *, *, #1620, .F. ) ;
#14633 = EDGE_CURVE ( 'NONE', #6341, #11343, #15710, .T. ) ;
#14634 = AXIS2_PLACEMENT_3D ( 'NONE', #18688, #3540, #10272 ) ;
#14635 = VERTEX_POINT ( 'NONE', #11052 ) ;
#14636 = ORIENTED_EDGE ( 'NONE', *, *, #20676, .F. ) ;
#14637 = CIRCLE ( 'NONE', #867, 113.8250000000000028 ) ;
#14638 = ORIENTED_EDGE ( 'NONE', *, *, #20256, .T. ) ;
#14639 = DIRECTION ( 'NONE',  ( -1.000000000000000000, 0.000000000000000000, -0.000000000000000000 ) ) ;
#14640 = CARTESIAN_POINT ( 'NONE',  ( 10.00000000000000000, -85.05652083079338865, -0.7600687895868707411 ) ) ;
#14641 = ORIENTED_EDGE ( 'NONE', *, *, #12275, .F. ) ;
#14642 = AXIS2_PLACEMENT_3D ( 'NONE', #1517, #6835, #13559 ) ;
#14643 = DIRECTION ( 'NONE',  ( -1.000000000000000000, -0.000000000000000000, 0.000000000000000000 ) ) ;
#14644 = FACE_BOUND ( 'NONE', #11294, .T. ) ;
#14645 = CARTESIAN_POINT ( 'NONE',  ( -7.395799999999999486, 1.407128969394701661E-14, 114.9007999999999896 ) ) ;
#14646 = CARTESIAN_POINT ( 'NONE',  ( 0.000000000000000000, 0.000000000000000000, 0.000000000000000000 ) ) ;
#14647 = CIRCLE ( 'NONE', #12522, 44.99999999999999289 ) ;
#14648 = CARTESIAN_POINT ( 'NONE',  ( 10.00000000000000000, 56.35896156215049047, -73.34918167666251065 ) ) ;
#14649 = ORIENTED_EDGE ( 'NONE', *, *, #712, .F. ) ;
#14650 = CARTESIAN_POINT ( 'NONE',  ( 10.00000000000000000, 77.39385041987100067, 35.28996114464738554 ) ) ;
#14651 = DIRECTION ( 'NONE',  ( 0.000000000000000000, 2.929755203871941151E-14, -1.000000000000000000 ) ) ;
#14652 = ORIENTED_EDGE ( 'NONE', *, *, #15040, .F. ) ;
#14653 = AXIS2_PLACEMENT_3D ( 'NONE', #20744, #7153, #13887 ) ;
#14654 = AXIS2_PLACEMENT_3D ( 'NONE', #18290, #16618, #11313 ) ;
#14655 = AXIS2_PLACEMENT_3D ( 'NONE', #10459, #20423, #10344 ) ;
#14656 = CARTESIAN_POINT ( 'NONE',  ( 0.000000000000000000, -19.07277123396528040, -19.80970465344767817 ) ) ;
#14657 = AXIS2_PLACEMENT_3D ( 'NONE', #15259, #1797, #32 ) ;
#14658 = ORIENTED_EDGE ( 'NONE', *, *, #15165, .T. ) ;
#14659 = CARTESIAN_POINT ( 'NONE',  ( 0.000000000000000000, -46.07110168784768689, -74.97635353408431058 ) ) ;
#14660 = CARTESIAN_POINT ( 'NONE',  ( 10.00000000000000000, 0.000000000000000000, 0.000000000000000000 ) ) ;
#14661 = ORIENTED_EDGE ( 'NONE', *, *, #8157, .F. ) ;
#14662 = CARTESIAN_POINT ( 'NONE',  ( 0.000000000000000000, -81.83745710415297481, 32.35167097270122838 ) ) ;
#14663 = VERTEX_POINT ( 'NONE', #20894 ) ;
#14664 = ORIENTED_EDGE ( 'NONE', *, *, #4449, .F. ) ;
#14665 = DIRECTION ( 'NONE',  ( -1.000000000000000000, 0.000000000000000000, 0.000000000000000000 ) ) ;
#14666 = ORIENTED_EDGE ( 'NONE', *, *, #8700, .T. ) ;
#14667 = CARTESIAN_POINT ( 'NONE',  ( 0.000000000000000000, 92.49798535263882115, 0.7467976319023850174 ) ) ;
#14668 = CARTESIAN_POINT ( 'NONE',  ( 10.00000000000000000, 15.32665449651924661, 91.22241316115426457 ) ) ;
#14669 = DIRECTION ( 'NONE',  ( 0.000000000000000000, 0.000000000000000000, -1.000000000000000000 ) ) ;
#14670 = AXIS2_PLACEMENT_3D ( 'NONE', #15193, #7531, #17494 ) ;
#14671 = AXIS2_PLACEMENT_3D ( 'NONE', #13973, #8989, #10547 ) ;
#14672 = CARTESIAN_POINT ( 'NONE',  ( 10.00000000000000000, 0.000000000000000000, 0.000000000000000000 ) ) ;
#14673 = CIRCLE ( 'NONE', #4093, 92.50100000000000477 ) ;
#14674 = AXIS2_PLACEMENT_3D ( 'NONE', #1113, #11169, #14223 ) ;
#14675 = CARTESIAN_POINT ( 'NONE',  ( 0.000000000000000000, 0.000000000000000000, 0.000000000000000000 ) ) ;
#14676 = DIRECTION ( 'NONE',  ( 0.000000000000000000, -0.8987940462991711454, 0.4383711467890689661 ) ) ;
#14677 = CARTESIAN_POINT ( 'NONE',  ( 0.000000000000000000, 0.000000000000000000, 0.000000000000000000 ) ) ;
#14678 = CARTESIAN_POINT ( 'NONE',  ( 0.000000000000000000, 52.96496548042853192, 66.55750800669373746 ) ) ;
#14679 = CARTESIAN_POINT ( 'NONE',  ( 0.000000000000000000, 25.56104204395304080, 81.12843256239672485 ) ) ;
#14680 = DIRECTION ( 'NONE',  ( 0.000000000000000000, 0.000000000000000000, 1.000000000000000000 ) ) ;
#14681 = ORIENTED_EDGE ( 'NONE', *, *, #12557, .T. ) ;
#14682 = EDGE_CURVE ( 'NONE', #14906, #18352, #6663, .T. ) ;
#14683 = CIRCLE ( 'NONE', #4452, 44.99999999999999289 ) ;
#14684 = ORIENTED_EDGE ( 'NONE', *, *, #2843, .F. ) ;
#14685 = AXIS2_PLACEMENT_3D ( 'NONE', #11081, #12842, #15943 ) ;
#14686 = VERTEX_POINT ( 'NONE', #14152 ) ;
#14687 = EDGE_LOOP ( 'NONE', ( #10592, #15479, #12913, #14921 ) ) ;
#14688 = EDGE_CURVE ( 'NONE', #13148, #7101, #20765, .T. ) ;
#14689 = EDGE_LOOP ( 'NONE', ( #403, #12975, #20158, #17810 ) ) ;
#14690 = CARTESIAN_POINT ( 'NONE',  ( 10.00000000000000000, 60.65279801375431390, -63.75921967137554702 ) ) ;
#14691 = ORIENTED_EDGE ( 'NONE', *, *, #13130, .T. ) ;
#14692 = DIRECTION ( 'NONE',  ( -1.000000000000000000, 0.000000000000000000, 0.000000000000000000 ) ) ;
#14693 = DIRECTION ( 'NONE',  ( 0.000000000000000000, 0.4067366430758010409, -0.9135454576426005335 ) ) ;
#14694 = DIRECTION ( 'NONE',  ( 0.000000000000000000, 0.000000000000000000, -1.000000000000000000 ) ) ;
#14695 = AXIS2_PLACEMENT_3D ( 'NONE', #15515, #10428, #17067 ) ;
#14696 = DIRECTION ( 'NONE',  ( -1.000000000000000000, -0.000000000000000000, -0.000000000000000000 ) ) ;
#14697 = TOROIDAL_SURFACE ( 'NONE', #18932, 6.866799999999992465, 0.02570000000000154800 ) ;
#14698 = CARTESIAN_POINT ( 'NONE',  ( 10.00000000000000000, 8.925965667928872804, 92.06933331948788179 ) ) ;
#14699 = CIRCLE ( 'NONE', #19646, 11.99999999999999822 ) ;
#14700 = DIRECTION ( 'NONE',  ( -1.000000000000000000, -0.000000000000000000, -0.000000000000000000 ) ) ;
#14701 = CARTESIAN_POINT ( 'NONE',  ( 0.000000000000000000, 27.48365448817206769, 0.9185515634842894572 ) ) ;
#14702 = ORIENTED_EDGE ( 'NONE', *, *, #6891, .T. ) ;
#14703 = LINE ( 'NONE', #16028, #13246 ) ;
#14704 = EDGE_CURVE ( 'NONE', #239, #21406, #17486, .T. ) ;
#14705 = EDGE_CURVE ( 'NONE', #12763, #15688, #12287, .T. ) ;
#14706 = ORIENTED_EDGE ( 'NONE', *, *, #6496, .F. ) ;
#14707 = EDGE_LOOP ( 'NONE', ( #21085, #6773, #4113, #15043 ) ) ;
#14708 = CARTESIAN_POINT ( 'NONE',  ( 10.00000000000000000, 69.25892805976580746, -49.38005998797770246 ) ) ;
#14709 = AXIS2_PLACEMENT_3D ( 'NONE', #441, #7180, #16916 ) ;
#14710 = EDGE_CURVE ( 'NONE', #7036, #20191, #15111, .T. ) ;
#14711 = CARTESIAN_POINT ( 'NONE',  ( -10.00000000000000000, 0.000000000000000000, 0.000000000000000000 ) ) ;
#14712 = VERTEX_POINT ( 'NONE', #1011 ) ;
#14713 = AXIS2_PLACEMENT_3D ( 'NONE', #6491, #8356, #10001 ) ;
#14714 = LINE ( 'NONE', #21458, #4535 ) ;
#14715 = VERTEX_POINT ( 'NONE', #10840 ) ;
#14716 = VERTEX_POINT ( 'NONE', #17592 ) ;
#14717 = AXIS2_PLACEMENT_3D ( 'NONE', #8931, #21094, #15676 ) ;
#14718 = DIRECTION ( 'NONE',  ( -0.9736356854027480301, -2.046083087085961801E-17, 0.2281086410251068064 ) ) ;
#14719 = DIRECTION ( 'NONE',  ( -1.000000000000000000, -0.000000000000000000, 0.000000000000000000 ) ) ;
#14720 = ORIENTED_EDGE ( 'NONE', *, *, #21618, .T. ) ;
#14721 = ORIENTED_EDGE ( 'NONE', *, *, #18243, .T. ) ;
#14722 = DIRECTION ( 'NONE',  ( -1.000000000000000000, 0.000000000000000000, 0.000000000000000000 ) ) ;
#14723 = FACE_OUTER_BOUND ( 'NONE', #18725, .T. ) ;
#14724 = ADVANCED_FACE ( 'NONE', ( #2452 ), #14377, .T. ) ;
#14725 = DIRECTION ( 'NONE',  ( -1.000000000000000000, 0.000000000000000000, 0.000000000000000000 ) ) ;
#14726 = DIRECTION ( 'NONE',  ( 0.000000000000000000, -6.982962677686266711E-15, 1.000000000000000000 ) ) ;
#14727 = SURFACE_SIDE_STYLE ('',( #13168 ) ) ;
#14728 = DIRECTION ( 'NONE',  ( 1.000000000000000000, 0.000000000000000000, 0.000000000000000000 ) ) ;
#14729 = LINE ( 'NONE', #18055, #19895 ) ;
#14730 = ADVANCED_FACE ( 'NONE', ( #12387 ), #780, .T. ) ;
#14731 = DIRECTION ( 'NONE',  ( -1.000000000000000000, -0.000000000000000000, 0.000000000000000000 ) ) ;
#14732 = DIRECTION ( 'NONE',  ( 0.000000000000000000, 0.000000000000000000, 1.000000000000000000 ) ) ;
#14733 = VECTOR ( 'NONE', #17675, 1000.000000000000000 ) ;
#14734 = CIRCLE ( 'NONE', #21779, 27.49900000000000233 ) ;
#14735 = VERTEX_POINT ( 'NONE', #2544 ) ;
#14736 = AXIS2_PLACEMENT_3D ( 'NONE', #313, #18759, #20098 ) ;
#14737 = EDGE_CURVE ( 'NONE', #10208, #17938, #16540, .T. ) ;
#14738 = ORIENTED_EDGE ( 'NONE', *, *, #10282, .T. ) ;
#14739 = EDGE_CURVE ( 'NONE', #12821, #19022, #12644, .T. ) ;
#14740 = CYLINDRICAL_SURFACE ( 'NONE', #13698, 45.00000000000000000 ) ;
#14741 = ADVANCED_FACE ( 'NONE', ( #19676 ), #1339, .F. ) ;
#14742 = SURFACE_STYLE_FILL_AREA ( #6033 ) ;
#14743 = DIRECTION ( 'NONE',  ( 1.000000000000000000, -0.000000000000000000, -0.000000000000000000 ) ) ;
#14744 = ORIENTED_EDGE ( 'NONE', *, *, #13881, .F. ) ;
#14745 = AXIS2_PLACEMENT_3D ( 'NONE', #10068, #16817, #1685 ) ;
#14746 = VECTOR ( 'NONE', #4014, 1000.000000000000000 ) ;
#14747 = ORIENTED_EDGE ( 'NONE', *, *, #16209, .T. ) ;
#14748 = ORIENTED_EDGE ( 'NONE', *, *, #21201, .F. ) ;
#14749 = CIRCLE ( 'NONE', #5572, 92.50100000000001899 ) ;
#14750 = ORIENTED_EDGE ( 'NONE', *, *, #17489, .T. ) ;
#14751 = VECTOR ( 'NONE', #12224, 1000.000000000000000 ) ;
#14752 = FACE_OUTER_BOUND ( 'NONE', #14707, .T. ) ;
#14753 = CARTESIAN_POINT ( 'NONE',  ( 10.00000000000000000, 15.32665449652044920, -91.22241316115403720 ) ) ;
#14754 = CIRCLE ( 'NONE', #15806, 44.99999999999999289 ) ;
#14755 = VERTEX_POINT ( 'NONE', #2880 ) ;
#14756 = ADVANCED_FACE ( 'NONE', ( #1551 ), #6655, .T. ) ;
#14757 = DIRECTION ( 'NONE',  ( 0.000000000000000000, 0.000000000000000000, 1.000000000000000000 ) ) ;
#14758 = DIRECTION ( 'NONE',  ( 1.000000000000000000, 0.000000000000000000, 0.000000000000000000 ) ) ;
#14759 = CARTESIAN_POINT ( 'NONE',  ( 10.00000000000000000, -86.66425444033897918, -32.33793443156484670 ) ) ;
#14760 = EDGE_CURVE ( 'NONE', #17965, #9285, #9505, .T. ) ;
#14761 = FACE_OUTER_BOUND ( 'NONE', #18432, .T. ) ;
#14762 = AXIS2_PLACEMENT_3D ( 'NONE', #776, #5878, #10835 ) ;
#14763 = CYLINDRICAL_SURFACE ( 'NONE', #9276, 44.99999999999999289 ) ;
#14764 = DIRECTION ( 'NONE',  ( -1.000000000000000000, 0.000000000000000000, 0.000000000000000000 ) ) ;
#14765 = APPLICATION_CONTEXT ( 'automotive_design' ) ;
#14766 = ORIENTED_EDGE ( 'NONE', *, *, #16740, .T. ) ;
#14767 = ADVANCED_FACE ( 'NONE', ( #18254 ), #9716, .F. ) ;
#14768 = DIRECTION ( 'NONE',  ( 0.000000000000000000, 0.000000000000000000, -1.000000000000000000 ) ) ;
#14769 = AXIS2_PLACEMENT_3D ( 'NONE', #3880, #3654, #10614 ) ;
#14770 = CARTESIAN_POINT ( 'NONE',  ( 0.000000000000000000, 13.56333590714055326, -28.98337314858420299 ) ) ;
#14771 = VECTOR ( 'NONE', #15559, 1000.000000000000000 ) ;
#14772 = ORIENTED_EDGE ( 'NONE', *, *, #5385, .T. ) ;
#14773 = CIRCLE ( 'NONE', #17251, 88.00000000000000000 ) ;
#14774 = CIRCLE ( 'NONE', #11234, 88.00000000000000000 ) ;
#14775 = DIRECTION ( 'NONE',  ( -1.000000000000000000, 0.000000000000000000, 0.000000000000000000 ) ) ;
#14776 = ORIENTED_EDGE ( 'NONE', *, *, #15183, .T. ) ;
#14777 = EDGE_CURVE ( 'NONE', #845, #11182, #15476, .T. ) ;
#14778 = FACE_OUTER_BOUND ( 'NONE', #18728, .T. ) ;
#14779 = CARTESIAN_POINT ( 'NONE',  ( 0.000000000000000000, 0.000000000000000000, 0.000000000000000000 ) ) ;
#14780 = ORIENTED_EDGE ( 'NONE', *, *, #15427, .T. ) ;
#14781 = DIRECTION ( 'NONE',  ( -1.000000000000000000, -0.000000000000000000, 0.000000000000000000 ) ) ;
#14782 = ORIENTED_EDGE ( 'NONE', *, *, #10115, .T. ) ;
#14783 = ORIENTED_EDGE ( 'NONE', *, *, #9584, .T. ) ;
#14784 = DIRECTION ( 'NONE',  ( 0.000000000000000000, 0.000000000000000000, 1.000000000000000000 ) ) ;
#14785 = VERTEX_POINT ( 'NONE', #14701 ) ;
#14786 = DIRECTION ( 'NONE',  ( 1.000000000000000000, 0.000000000000000000, 0.000000000000000000 ) ) ;
#14787 = AXIS2_PLACEMENT_3D ( 'NONE', #7607, #20974, #15780 ) ;
#14788 = CARTESIAN_POINT ( 'NONE',  ( 0.000000000000000000, 0.000000000000000000, 0.000000000000000000 ) ) ;
#14789 = DIRECTION ( 'NONE',  ( 1.000000000000000000, 0.000000000000000000, 0.000000000000000000 ) ) ;
#14790 = CIRCLE ( 'NONE', #5262, 88.00000000000000000 ) ;
#14791 = VECTOR ( 'NONE', #7706, 1000.000000000000000 ) ;
#14792 = AXIS2_PLACEMENT_3D ( 'NONE', #17676, #7617, #11028 ) ;
#14793 = SURFACE_STYLE_USAGE ( .BOTH. , #1312 ) ;
#14794 = DIRECTION ( 'NONE',  ( 0.000000000000000000, 0.5877852522924689183, 0.8090169943749504489 ) ) ;
#14795 = FACE_OUTER_BOUND ( 'NONE', #15589, .T. ) ;
#14796 = EDGE_CURVE ( 'NONE', #12932, #21704, #8773, .T. ) ;
#14797 = CARTESIAN_POINT ( 'NONE',  ( 0.000000000000000000, 0.000000000000000000, 0.000000000000000000 ) ) ;
#14798 = CARTESIAN_POINT ( 'NONE',  ( 10.00000000000000000, 0.000000000000000000, 0.000000000000000000 ) ) ;
#14799 = CYLINDRICAL_SURFACE ( 'NONE', #15692, 11.99999999999999822 ) ;
#14800 = FACE_OUTER_BOUND ( 'NONE', #5731, .T. ) ;
#14801 = VECTOR ( 'NONE', #913, 1000.000000000000000 ) ;
#14802 = ORIENTED_EDGE ( 'NONE', *, *, #9428, .F. ) ;
#14803 = ORIENTED_EDGE ( 'NONE', *, *, #1491, .T. ) ;
#14804 = AXIS2_PLACEMENT_3D ( 'NONE', #15324, #11911, #16995 ) ;
#14805 = VERTEX_POINT ( 'NONE', #12930 ) ;
#14806 = VERTEX_POINT ( 'NONE', #4546 ) ;
#14807 = ORIENTED_EDGE ( 'NONE', *, *, #2550, .T. ) ;
#14808 = DIRECTION ( 'NONE',  ( 1.000000000000000000, 0.000000000000000000, 0.000000000000000000 ) ) ;
#14809 = ORIENTED_EDGE ( 'NONE', *, *, #11447, .T. ) ;
#14810 = DIRECTION ( 'NONE',  ( 0.000000000000000000, 0.000000000000000000, -1.000000000000000000 ) ) ;
#14811 = DIRECTION ( 'NONE',  ( 1.000000000000000000, -0.000000000000000000, -0.000000000000000000 ) ) ;
#14812 = DIRECTION ( 'NONE',  ( 0.000000000000000000, 0.6427876096865405842, -0.7660444431189771253 ) ) ;
#14813 = DIRECTION ( 'NONE',  ( 0.000000000000000000, 0.5877852522924742473, -0.8090169943749466741 ) ) ;
#14814 = FACE_OUTER_BOUND ( 'NONE', #16400, .T. ) ;
#14815 = VECTOR ( 'NONE', #13409, 1000.000000000000000 ) ;
#14816 = CYLINDRICAL_SURFACE ( 'NONE', #18603, 11.99999999999999822 ) ;
#14817 = DIRECTION ( 'NONE',  ( 1.000000000000000000, 0.000000000000000000, 0.000000000000000000 ) ) ;
#14818 = ORIENTED_EDGE ( 'NONE', *, *, #6537, .T. ) ;
#14819 = EDGE_CURVE ( 'NONE', #9851, #10156, #13344, .T. ) ;
#14820 = CYLINDRICAL_SURFACE ( 'NONE', #19990, 32.00000000000000000 ) ;
#14821 = ORIENTED_EDGE ( 'NONE', *, *, #18160, .F. ) ;
#14822 = VERTEX_POINT ( 'NONE', #13045 ) ;
#14823 = DIRECTION ( 'NONE',  ( -1.000000000000000000, 0.000000000000000000, 0.000000000000000000 ) ) ;
#14824 = VERTEX_POINT ( 'NONE', #21658 ) ;
#14825 = AXIS2_PLACEMENT_3D ( 'NONE', #8309, #15039, #11723 ) ;
#14826 = CARTESIAN_POINT ( 'NONE',  ( 10.00000000000000000, 64.66851233300799606, -55.25552418572899427 ) ) ;
#14827 = ORIENTED_EDGE ( 'NONE', *, *, #13929, .F. ) ;
#14828 = ORIENTED_EDGE ( 'NONE', *, *, #18657, .F. ) ;
#14829 = DIRECTION ( 'NONE',  ( 0.000000000000000000, -9.772275581336014350E-15, -1.000000000000000000 ) ) ;
#14830 = ORIENTED_EDGE ( 'NONE', *, *, #16507, .T. ) ;
#14831 = DIRECTION ( 'NONE',  ( 0.000000000000000000, 0.000000000000000000, -1.000000000000000000 ) ) ;
#14832 = DIRECTION ( 'NONE',  ( 0.000000000000000000, 0.9510565162951521989, 0.3090169943749514481 ) ) ;
#14833 = DIRECTION ( 'NONE',  ( -1.000000000000000000, 0.000000000000000000, 0.000000000000000000 ) ) ;
#14834 = CARTESIAN_POINT ( 'NONE',  ( 10.00000000000000000, -41.89587599971600440, 77.38692120905457728 ) ) ;
#14835 = ADVANCED_FACE ( 'NONE', ( #11715 ), #11284, .F. ) ;
#14836 = DIRECTION ( 'NONE',  ( 0.000000000000000000, 0.000000000000000000, 1.000000000000000000 ) ) ;
#14837 = CARTESIAN_POINT ( 'NONE',  ( 10.00000000000000000, 19.83954325428771881, -82.71385593638672162 ) ) ;
#14838 = DIRECTION ( 'NONE',  ( -1.000000000000000000, -0.000000000000000000, -0.000000000000000000 ) ) ;
#14839 = DIRECTION ( 'NONE',  ( -1.000000000000000000, -0.000000000000000000, 0.000000000000000000 ) ) ;
#14840 = CARTESIAN_POINT ( 'NONE',  ( -1.200000000000006617, 6.873330160214519262E-16, 5.612499999999999822 ) ) ;
#14841 = VECTOR ( 'NONE', #2735, 1000.000000000000000 ) ;
#14842 = ORIENTED_EDGE ( 'NONE', *, *, #4622, .F. ) ;
#14843 = EDGE_CURVE ( 'NONE', #18019, #8212, #17238, .T. ) ;
#14844 = ORIENTED_EDGE ( 'NONE', *, *, #21396, .T. ) ;
#14845 = FACE_OUTER_BOUND ( 'NONE', #10958, .T. ) ;
#14846 = EDGE_CURVE ( 'NONE', #12774, #19231, #5594, .T. ) ;
#14847 = DIRECTION ( 'NONE',  ( 1.000000000000000000, 0.000000000000000000, 0.000000000000000000 ) ) ;
#14848 = ORIENTED_EDGE ( 'NONE', *, *, #410, .T. ) ;
#14849 = AXIS2_PLACEMENT_3D ( 'NONE', #11438, #9892, #19950 ) ;
#14850 = CARTESIAN_POINT ( 'NONE',  ( 5.000000000000000000, -68.93609746931124960, -54.69748134696530428 ) ) ;
#14851 = ORIENTED_EDGE ( 'NONE', *, *, #8255, .T. ) ;
#14852 = SHAPE_REPRESENTATION_RELATIONSHIP ( 'NONE' , 'NONE' ,  #11927, #7762 ) ;
#14853 = EDGE_LOOP ( 'NONE', ( #1242, #21160, #5840, #14341 ) ) ;
#14854 = DIRECTION ( 'NONE',  ( 0.000000000000000000, 0.9993908270190956511, 0.03489949670250451497 ) ) ;
#14855 = VERTEX_POINT ( 'NONE', #11382 ) ;
#14856 = ORIENTED_EDGE ( 'NONE', *, *, #7042, .F. ) ;
#14857 = AXIS2_PLACEMENT_3D ( 'NONE', #3277, #297, #6611 ) ;
#14858 = CARTESIAN_POINT ( 'NONE',  ( 0.000000000000000000, 0.000000000000000000, 0.000000000000000000 ) ) ;
#14859 = DIRECTION ( 'NONE',  ( 1.000000000000000000, 0.000000000000000000, 0.000000000000000000 ) ) ;
#14860 = ORIENTED_EDGE ( 'NONE', *, *, #20918, .T. ) ;
#14861 = EDGE_CURVE ( 'NONE', #1477, #4091, #6435, .T. ) ;
#14862 = CARTESIAN_POINT ( 'NONE',  ( 1.500000000000000000, 15.00000000000000000, 7.000000000000000000 ) ) ;
#14863 = CARTESIAN_POINT ( 'NONE',  ( 10.00000000000000000, -74.39348546125087580, 54.97312363261389834 ) ) ;
#14864 = EDGE_CURVE ( 'NONE', #3479, #750, #14416, .T. ) ;
#14865 = CARTESIAN_POINT ( 'NONE',  ( 10.00000000000000000, 23.10190250628953379, -89.56973317806578905 ) ) ;
#14866 = EDGE_CURVE ( 'NONE', #3599, #17431, #4901, .T. ) ;
#14867 = CARTESIAN_POINT ( 'NONE',  ( 0.000000000000000000, -84.80486432185219314, 36.94008646920367056 ) ) ;
#14868 = CARTESIAN_POINT ( 'NONE',  ( 0.000000000000000000, 75.27139873020959726, -53.76477968147737840 ) ) ;
#14869 = DIRECTION ( 'NONE',  ( -1.000000000000000000, -0.000000000000000000, 0.000000000000000000 ) ) ;
#14870 = EDGE_CURVE ( 'NONE', #11727, #14824, #21476, .T. ) ;
#14871 = ORIENTED_EDGE ( 'NONE', *, *, #7136, .F. ) ;
#14872 = CARTESIAN_POINT ( 'NONE',  ( 10.00000000000000000, -84.33453774737651543, -11.08490790852216534 ) ) ;
#14873 = DIRECTION ( 'NONE',  ( 1.000000000000000000, 0.000000000000000000, 0.000000000000000000 ) ) ;
#14874 = VERTEX_POINT ( 'NONE', #20125 ) ;
#14875 = ADVANCED_BREP_SHAPE_REPRESENTATION ( '', ( #20649, #15567 ), #3925 ) ;
#14876 = CARTESIAN_POINT ( 'NONE',  ( 7.440711023145912151, 0.000000000000000000, -104.9000000000000341 ) ) ;
#14877 = EDGE_CURVE ( 'NONE', #9931, #20811, #4981, .T. ) ;
#14878 = VERTEX_POINT ( 'NONE', #18464 ) ;
#14879 = FACE_OUTER_BOUND ( 'NONE', #7601, .T. ) ;
#14880 = CARTESIAN_POINT ( 'NONE',  ( 0.000000000000000000, 0.000000000000000000, 0.000000000000000000 ) ) ;
#14881 = ORIENTED_EDGE ( 'NONE', *, *, #18160, .T. ) ;
#14882 = DIRECTION ( 'NONE',  ( -1.000000000000000000, 0.000000000000000000, -0.000000000000000000 ) ) ;
#14883 = ADVANCED_FACE ( 'NONE', ( #9832 ), #16584, .F. ) ;
#14884 = VERTEX_POINT ( 'NONE', #18899 ) ;
#14885 = ORIENTED_EDGE ( 'NONE', *, *, #16071, .T. ) ;
#14886 = LINE ( 'NONE', #19525, #11107 ) ;
#14887 = EDGE_CURVE ( 'NONE', #21758, #17790, #20226, .T. ) ;
#14888 = ORIENTED_EDGE ( 'NONE', *, *, #9306, .T. ) ;
#14889 = DIRECTION ( 'NONE',  ( -1.000000000000000000, -0.000000000000000000, -0.000000000000000000 ) ) ;
#14890 = DIRECTION ( 'NONE',  ( 1.000000000000000000, 0.000000000000000000, 0.000000000000000000 ) ) ;
#14891 = CARTESIAN_POINT ( 'NONE',  ( -90.00000000000000000, 0.000000000000000000, 0.000000000000000000 ) ) ;
#14892 = DIRECTION ( 'NONE',  ( 0.000000000000000000, 0.000000000000000000, -1.000000000000000000 ) ) ;
#14893 = CARTESIAN_POINT ( 'NONE',  ( -1.399999999999998579, 0.000000000000000000, 0.000000000000000000 ) ) ;
#14894 = EDGE_CURVE ( 'NONE', #536, #6705, #1367, .T. ) ;
#14895 = CARTESIAN_POINT ( 'NONE',  ( 10.00000000000000000, -17.83210509884655792, 21.83428559348755371 ) ) ;
#14896 = CARTESIAN_POINT ( 'NONE',  ( 10.00000000000000000, 27.07404830566976983, -4.815694066514164540 ) ) ;
#14897 = CARTESIAN_POINT ( 'NONE',  ( 0.000000000000000000, 24.89070495400735794, 84.40647372620510680 ) ) ;
#14898 = AXIS2_PLACEMENT_3D ( 'NONE', #6856, #9934, #13139 ) ;
#14899 = DIRECTION ( 'NONE',  ( -1.000000000000000000, -0.000000000000000000, -0.000000000000000000 ) ) ;
#14900 = CARTESIAN_POINT ( 'NONE',  ( 0.000000000000000000, 0.000000000000000000, 0.000000000000000000 ) ) ;
#14901 = EDGE_CURVE ( 'NONE', #16742, #15174, #4186, .T. ) ;
#14902 = VERTEX_POINT ( 'NONE', #14 ) ;
#14903 = ORIENTED_EDGE ( 'NONE', *, *, #18415, .T. ) ;
#14904 = EDGE_CURVE ( 'NONE', #20733, #18352, #19357, .T. ) ;
#14905 = ORIENTED_EDGE ( 'NONE', *, *, #3390, .F. ) ;
#14906 = VERTEX_POINT ( 'NONE', #7087 ) ;
#14907 = EDGE_CURVE ( 'NONE', #3553, #8843, #12305, .T. ) ;
#14908 = ADVANCED_FACE ( 'NONE', ( #13913 ), #13706, .F. ) ;
#14909 = ORIENTED_EDGE ( 'NONE', *, *, #19078, .F. ) ;
#14910 = DIRECTION ( 'NONE',  ( 0.000000000000000000, 0.000000000000000000, 1.000000000000000000 ) ) ;
#14911 = EDGE_LOOP ( 'NONE', ( #11008, #15655, #19460, #18519 ) ) ;
#14912 = DIRECTION ( 'NONE',  ( 0.000000000000000000, 0.000000000000000000, 1.000000000000000000 ) ) ;
#14913 = DIRECTION ( 'NONE',  ( -0.000000000000000000, 0.000000000000000000, 1.000000000000000000 ) ) ;
#14914 = AXIS2_PLACEMENT_3D ( 'NONE', #18442, #3294, #10022 ) ;
#14915 = CARTESIAN_POINT ( 'NONE',  ( 10.00000000000000000, 19.85071254963777676, 20.01672328094538145 ) ) ;
#14916 = CARTESIAN_POINT ( 'NONE',  ( -10.00000000000000000, 0.000000000000000000, 0.000000000000000000 ) ) ;
#14917 = DIRECTION ( 'NONE',  ( 1.000000000000000000, 0.000000000000000000, 0.000000000000000000 ) ) ;
#14918 = CARTESIAN_POINT ( 'NONE',  ( 10.00000000000000000, 83.03980459022480431, -18.42770452393272862 ) ) ;
#14919 = DIRECTION ( 'NONE',  ( -1.000000000000000000, -0.000000000000000000, -0.000000000000000000 ) ) ;
#14920 = CIRCLE ( 'NONE', #15972, 92.50099999999999056 ) ;
#14921 = ORIENTED_EDGE ( 'NONE', *, *, #12404, .T. ) ;
#14922 = DIRECTION ( 'NONE',  ( 0.000000000000000000, -0.2079116908177666145, 0.9781476007338040235 ) ) ;
#14923 = AXIS2_PLACEMENT_3D ( 'NONE', #15570, #19108, #14234 ) ;
#14924 = CIRCLE ( 'NONE', #16688, 10.49999999999999822 ) ;
#14925 = ORIENTED_EDGE ( 'NONE', *, *, #272, .F. ) ;
#14926 = CIRCLE ( 'NONE', #17410, 88.00000000000000000 ) ;
#14927 = VERTEX_POINT ( 'NONE', #20455 ) ;
#14928 = CARTESIAN_POINT ( 'NONE',  ( 1.199999999999992628, 0.000000000000000000, -6.887500000000022382 ) ) ;
#14929 = ORIENTED_EDGE ( 'NONE', *, *, #7446, .T. ) ;
#14930 = CARTESIAN_POINT ( 'NONE',  ( 0.000000000000000000, 83.03980459022454852, 18.42770452393382641 ) ) ;
#14931 = ORIENTED_EDGE ( 'NONE', *, *, #17427, .T. ) ;
#14932 = EDGE_LOOP ( 'NONE', ( #10585, #2864, #10875, #10286 ) ) ;
#14933 = CARTESIAN_POINT ( 'NONE',  ( 5.000000000000000888, 30.61448696004464409, -9.314139153633925972 ) ) ;
#14934 = CIRCLE ( 'NONE', #10688, 44.99999999999999289 ) ;
#14935 = EDGE_LOOP ( 'NONE', ( #10796, #13840, #4923, #1125 ) ) ;
#14936 = LINE ( 'NONE', #1985, #5801 ) ;
#14937 = CARTESIAN_POINT ( 'NONE',  ( 10.00000000000000000, -9.992993448021772807, 26.36019881529882980 ) ) ;
#14938 = CIRCLE ( 'NONE', #5424, 44.99999999999999289 ) ;
#14939 = FACE_OUTER_BOUND ( 'NONE', #7816, .T. ) ;
#14940 = DIRECTION ( 'NONE',  ( 1.000000000000000000, 0.000000000000000000, 0.000000000000000000 ) ) ;
#14941 = CIRCLE ( 'NONE', #17064, 44.99999999999999289 ) ;
#14942 = DIRECTION ( 'NONE',  ( 1.000000000000000000, 0.000000000000000000, -0.000000000000000000 ) ) ;
#14943 = DIRECTION ( 'NONE',  ( 0.000000000000000000, 0.000000000000000000, 1.000000000000000000 ) ) ;
#14944 = DIRECTION ( 'NONE',  ( 0.000000000000000000, 0.7431448254773953543, -0.6691306063588569053 ) ) ;
#14945 = ORIENTED_EDGE ( 'NONE', *, *, #14180, .T. ) ;
#14946 = CIRCLE ( 'NONE', #6151, 7.400000000000020783 ) ;
#14947 = DIRECTION ( 'NONE',  ( -1.000000000000000000, 0.000000000000000000, -0.000000000000000000 ) ) ;
#14948 = DIRECTION ( 'NONE',  ( 0.000000000000000000, 0.000000000000000000, 1.000000000000000000 ) ) ;
#14949 = ORIENTED_EDGE ( 'NONE', *, *, #5560, .T. ) ;
#14950 = ADVANCED_FACE ( 'NONE', ( #6761 ), #1669, .F. ) ;
#14951 = DIRECTION ( 'NONE',  ( 1.000000000000000000, 0.000000000000000000, 0.000000000000000000 ) ) ;
#14952 = VERTEX_POINT ( 'NONE', #8410 ) ;
#14953 = CIRCLE ( 'NONE', #13899, 11.99999999999999822 ) ;
#14954 = EDGE_LOOP ( 'NONE', ( #14449, #14388, #18995, #16812 ) ) ;
#14955 = DIRECTION ( 'NONE',  ( 1.000000000000000000, -0.000000000000000000, -0.000000000000000000 ) ) ;
#14956 = ORIENTED_EDGE ( 'NONE', *, *, #12290, .F. ) ;
#14957 = VERTEX_POINT ( 'NONE', #5419 ) ;
#14958 = DIRECTION ( 'NONE',  ( 0.000000000000000000, 0.000000000000000000, 1.000000000000000000 ) ) ;
#14959 = CARTESIAN_POINT ( 'NONE',  ( 0.000000000000000000, 0.000000000000000000, 0.000000000000000000 ) ) ;
#14960 = EDGE_CURVE ( 'NONE', #20936, #14091, #7382, .T. ) ;
#14961 = VERTEX_POINT ( 'NONE', #1777 ) ;
#14962 = AXIS2_PLACEMENT_3D ( 'NONE', #277, #5148, #2146 ) ;
#14963 = CARTESIAN_POINT ( 'NONE',  ( 10.00000000000000000, -12.94633825542249994, -24.26081875733348170 ) ) ;
#14964 = PLANE ( 'NONE',  #10814 ) ;
#14965 = CARTESIAN_POINT ( 'NONE',  ( 0.000000000000000000, 0.000000000000000000, -3.000000000000000000 ) ) ;
#14966 = CARTESIAN_POINT ( 'NONE',  ( 10.00000000000000000, 13.56333590714014825, 28.98337314858439484 ) ) ;
#14967 = LINE ( 'NONE', #18308, #4704 ) ;
#14968 = DIRECTION ( 'NONE',  ( -1.000000000000000000, -0.000000000000000000, 0.000000000000000000 ) ) ;
#14969 = UNCERTAINTY_MEASURE_WITH_UNIT (LENGTH_MEASURE( 1.000000000000000082E-05 ), #17738, 'distance_accuracy_value', 'NONE');
#14970 = AXIS2_PLACEMENT_3D ( 'NONE', #12758, #17748, #3934 ) ;
#14971 = ORIENTED_EDGE ( 'NONE', *, *, #742, .F. ) ;
#14972 = CIRCLE ( 'NONE', #17462, 88.00000000000000000 ) ;
#14973 = CARTESIAN_POINT ( 'NONE',  ( 5.000000000000002665, -86.77540292929711541, 14.62974526292689426 ) ) ;
#14974 = DIRECTION ( 'NONE',  ( 1.000000000000000000, 0.000000000000000000, 0.000000000000000000 ) ) ;
#14975 = ORIENTED_EDGE ( 'NONE', *, *, #12179, .T. ) ;
#14976 = DIRECTION ( 'NONE',  ( -1.000000000000000000, -0.000000000000000000, -0.000000000000000000 ) ) ;
#14977 = EDGE_LOOP ( 'NONE', ( #19602, #13511, #16998, #18994 ) ) ;
#14978 = AXIS2_PLACEMENT_3D ( 'NONE', #4132, #17622, #2572 ) ;
#14979 = CARTESIAN_POINT ( 'NONE',  ( -1.139999999999998570, 8.422079734756228398E-16, 6.866799999999992465 ) ) ;
#14980 = EDGE_CURVE ( 'NONE', #12538, #13997, #10553, .T. ) ;
#14982 = ADVANCED_FACE ( 'NONE', ( #15136 ), #3434, .F. ) ;
#14981 = AXIS2_PLACEMENT_3D ( 'NONE', #9267, #459, #16015 ) ;
#14983 = EDGE_CURVE ( 'NONE', #8691, #6248, #10194, .T. ) ;
#14984 = LINE ( 'NONE', #10118, #20093 ) ;
#14985 = VERTEX_POINT ( 'NONE', #12256 ) ;
#14986 = CIRCLE ( 'NONE', #12159, 126.5000000000000000 ) ;
#14987 = DIRECTION ( 'NONE',  ( 1.000000000000000000, 0.000000000000000000, 0.000000000000000000 ) ) ;
#14988 = VECTOR ( 'NONE', #915, 1000.000000000000000 ) ;
#14989 = EDGE_CURVE ( 'NONE', #19418, #15166, #17269, .T. ) ;
#14990 = ORIENTED_EDGE ( 'NONE', *, *, #4508, .T. ) ;
#14991 = ORIENTED_EDGE ( 'NONE', *, *, #18244, .F. ) ;
#14992 = FACE_OUTER_BOUND ( 'NONE', #2839, .T. ) ;
#14993 = ORIENTED_EDGE ( 'NONE', *, *, #15533, .T. ) ;
#14994 = FACE_OUTER_BOUND ( 'NONE', #13777, .T. ) ;
#14995 = CARTESIAN_POINT ( 'NONE',  ( -1.399999999999998579, 0.000000000000000000, 0.000000000000000000 ) ) ;
#14996 = CARTESIAN_POINT ( 'NONE',  ( 10.00000000000000000, 83.03980459022480431, -18.42770452393272862 ) ) ;
#14997 = CARTESIAN_POINT ( 'NONE',  ( 0.000000000000000000, 40.72878876293147954, 78.00747250042462611 ) ) ;
#14998 = LINE ( 'NONE', #10460, #4701 ) ;
#14999 = ADVANCED_FACE ( 'NONE', ( #13590 ), #20346, .F. ) ;
#15000 = CARTESIAN_POINT ( 'NONE',  ( 10.00000000000000000, -91.70173545986510533, -12.13370160540135423 ) ) ;
#15001 = AXIS2_PLACEMENT_3D ( 'NONE', #18314, #1611, #6390 ) ;
#15002 = FACE_OUTER_BOUND ( 'NONE', #15062, .T. ) ;
#15003 = AXIS2_PLACEMENT_3D ( 'NONE', #4042, #7691, #20844 ) ;
#15004 = EDGE_CURVE ( 'NONE', #2555, #2849, #10275, .T. ) ;
#15005 = CARTESIAN_POINT ( 'NONE',  ( 10.00000000000000000, -65.83713140174766920, 58.39068529131174756 ) ) ;
#15006 = VECTOR ( 'NONE', #18481, 1000.000000000000000 ) ;
#15007 = CARTESIAN_POINT ( 'NONE',  ( 0.000000000000000000, 56.35896156215049047, -73.34918167666251065 ) ) ;
#15008 = CARTESIAN_POINT ( 'NONE',  ( 10.00000000000000000, -25.48117629651182270, -10.33947075754286793 ) ) ;
#15009 = ORIENTED_EDGE ( 'NONE', *, *, #19359, .T. ) ;
#15010 = DIRECTION ( 'NONE',  ( 1.000000000000000000, -0.000000000000000000, -0.000000000000000000 ) ) ;
#15011 = EDGE_CURVE ( 'NONE', #19408, #20730, #10899, .T. ) ;
#15012 = ORIENTED_EDGE ( 'NONE', *, *, #10807, .T. ) ;
#15013 = ORIENTED_EDGE ( 'NONE', *, *, #1508, .F. ) ;
#15014 = ADVANCED_FACE ( 'NONE', ( #7405 ), #12691, .T. ) ;
#15015 = ORIENTED_EDGE ( 'NONE', *, *, #7270, .F. ) ;
#15016 = CIRCLE ( 'NONE', #5496, 45.00000000000000000 ) ;
#15017 = CIRCLE ( 'NONE', #12884, 45.00000000000000000 ) ;
#15018 = CIRCLE ( 'NONE', #15731, 44.99999999999999289 ) ;
#15019 = ORIENTED_EDGE ( 'NONE', *, *, #4464, .T. ) ;
#15020 = AXIS2_PLACEMENT_3D ( 'NONE', #19241, #7640, #12385 ) ;
#15021 = DIRECTION ( 'NONE',  ( 0.000000000000000000, 0.000000000000000000, -1.000000000000000000 ) ) ;
#15022 = ORIENTED_EDGE ( 'NONE', *, *, #6650, .T. ) ;
#15023 = DIRECTION ( 'NONE',  ( 0.000000000000000000, 0.000000000000000000, 1.000000000000000000 ) ) ;
#15024 = LINE ( 'NONE', #20002, #13147 ) ;
#15025 = ADVANCED_FACE ( 'NONE', ( #12469 ), #19215, .F. ) ;
#15026 = DIRECTION ( 'NONE',  ( 1.000000000000000000, 0.000000000000000000, 0.000000000000000000 ) ) ;
#15027 = CARTESIAN_POINT ( 'NONE',  ( 0.000000000000000000, 60.65279801375431390, -63.75921967137554702 ) ) ;
#15028 = ADVANCED_FACE ( 'NONE', ( #19009 ), #19112, .F. ) ;
#15029 = CARTESIAN_POINT ( 'NONE',  ( 0.000000000000000000, -91.49386717542212466, -13.61276130277086693 ) ) ;
#15030 = DIRECTION ( 'NONE',  ( 0.000000000000000000, 0.000000000000000000, -1.000000000000000000 ) ) ;
#15031 = AXIS2_PLACEMENT_3D ( 'NONE', #18256, #11943, #3545 ) ;
#15032 = EDGE_CURVE ( 'NONE', #21406, #510, #18337, .T. ) ;
#15033 = ORIENTED_EDGE ( 'NONE', *, *, #15427, .F. ) ;
#15034 = CIRCLE ( 'NONE', #14685, 101.1000000000000369 ) ;
#15035 = EDGE_CURVE ( 'NONE', #1766, #21050, #21148, .T. ) ;
#15036 = CARTESIAN_POINT ( 'NONE',  ( 0.000000000000000000, 31.88200538760793634, 2.745493118647102548 ) ) ;
#15037 = EDGE_LOOP ( 'NONE', ( #7392, #14956, #15393, #14055 ) ) ;
#15038 = ORIENTED_EDGE ( 'NONE', *, *, #8824, .F. ) ;
#15039 = DIRECTION ( 'NONE',  ( 1.000000000000000000, 0.000000000000000000, 0.000000000000000000 ) ) ;
#15040 = EDGE_CURVE ( 'NONE', #14952, #14101, #20096, .T. ) ;
#15041 = ORIENTED_EDGE ( 'NONE', *, *, #10116, .F. ) ;
#15042 = CARTESIAN_POINT ( 'NONE',  ( 10.00000000000000000, -89.12061559554314272, -24.77803214283632727 ) ) ;
#15043 = ORIENTED_EDGE ( 'NONE', *, *, #15411, .T. ) ;
#15044 = VERTEX_POINT ( 'NONE', #2199 ) ;
#15045 = SHAPE_DEFINITION_REPRESENTATION ( #3320, #21798 ) ;
#15046 = DIRECTION ( 'NONE',  ( 0.000000000000000000, -0.9848077530122062440, -0.1736481776669404897 ) ) ;
#15047 = ORIENTED_EDGE ( 'NONE', *, *, #14630, .T. ) ;
#15048 = AXIS2_PLACEMENT_3D ( 'NONE', #16235, #14240, #11029 ) ;
#15049 = CARTESIAN_POINT ( 'NONE',  ( 2.799999999999996714, 60.00000000000000000, 9.999999999999998224 ) ) ;
#15050 = AXIS2_PLACEMENT_3D ( 'NONE', #13612, #11964, #10399 ) ;
#15051 = DIRECTION ( 'NONE',  ( -1.000000000000000000, 0.000000000000000000, 0.000000000000000000 ) ) ;
#15052 = FACE_OUTER_BOUND ( 'NONE', #15595, .T. ) ;
#15053 = FACE_OUTER_BOUND ( 'NONE', #18700, .T. ) ;
#15054 = CARTESIAN_POINT ( 'NONE',  ( 0.000000000000000000, -51.76708072107842185, -67.49339815138544907 ) ) ;
#15055 = DIRECTION ( 'NONE',  ( -1.000000000000000000, 0.000000000000000000, 0.000000000000000000 ) ) ;
#15056 = CYLINDRICAL_SURFACE ( 'NONE', #18986, 45.00000000000000000 ) ;
#15057 = VERTEX_POINT ( 'NONE', #10703 ) ;
#15058 = AXIS2_PLACEMENT_3D ( 'NONE', #17920, #7641, #2543 ) ;
#15059 = VECTOR ( 'NONE', #110, 1000.000000000000000 ) ;
#15060 = DIRECTION ( 'NONE',  ( -1.000000000000000000, -0.000000000000000000, 0.000000000000000000 ) ) ;
#15061 = CARTESIAN_POINT ( 'NONE',  ( 10.00000000000000000, -5.479102470011078196, 87.82926298292112222 ) ) ;
#15062 = EDGE_LOOP ( 'NONE', ( #19610, #11881, #3066, #7838 ) ) ;
#15063 = DIRECTION ( 'NONE',  ( 0.000000000000000000, 0.000000000000000000, -1.000000000000000000 ) ) ;
#15064 = ORIENTED_EDGE ( 'NONE', *, *, #13286, .T. ) ;
#15065 = EDGE_LOOP ( 'NONE', ( #11812, #20606, #12616, #11680 ) ) ;
#15066 = DIRECTION ( 'NONE',  ( 0.000000000000000000, 0.000000000000000000, 1.000000000000000000 ) ) ;
#15067 = ORIENTED_EDGE ( 'NONE', *, *, #10580, .F. ) ;
#15068 = ORIENTED_EDGE ( 'NONE', *, *, #3409, .F. ) ;
#15069 = DIRECTION ( 'NONE',  ( -0.000000000000000000, -1.000000000000000000, -0.000000000000000000 ) ) ;
#15070 = VERTEX_POINT ( 'NONE', #3971 ) ;
#15071 = EDGE_LOOP ( 'NONE', ( #2949, #7221, #8005, #13404 ) ) ;
#15072 = CARTESIAN_POINT ( 'NONE',  ( 0.000000000000000000, 72.58367602204188529, 49.75550195834890843 ) ) ;
#15073 = CARTESIAN_POINT ( 'NONE',  ( 9.999999999999998224, 1.224646799147353059E-15, 15.00000000000000000 ) ) ;
#15074 = CARTESIAN_POINT ( 'NONE',  ( 0.000000000000000000, 91.49386717542222414, 13.61276130277023810 ) ) ;
#15075 = CARTESIAN_POINT ( 'NONE',  ( -90.00000000000000000, 1.409568465818603827E-14, 115.1000000000000227 ) ) ;
#15076 = AXIS2_PLACEMENT_3D ( 'NONE', #12116, #9304, #14288 ) ;
#15077 = CARTESIAN_POINT ( 'NONE',  ( 10.00000000000000000, -26.27606311335944511, -10.21217444509438188 ) ) ;
#15078 = FACE_OUTER_BOUND ( 'NONE', #20380, .T. ) ;
#15079 = VECTOR ( 'NONE', #4160, 1000.000000000000000 ) ;
#15080 = EDGE_CURVE ( 'NONE', #3591, #10715, #20077, .T. ) ;
#15081 = ORIENTED_EDGE ( 'NONE', *, *, #11271, .F. ) ;
#15082 = DIRECTION ( 'NONE',  ( -1.000000000000000000, 0.000000000000000000, -0.000000000000000000 ) ) ;
#15083 = DIRECTION ( 'NONE',  ( -1.000000000000000000, -0.000000000000000000, -0.000000000000000000 ) ) ;
#15084 = EDGE_LOOP ( 'NONE', ( #18644, #12942, #11479, #9728 ) ) ;
#15085 = PRODUCT_RELATED_PRODUCT_CATEGORY ( 'part', '', ( #1745 ) ) ;
#15086 = DIRECTION ( 'NONE',  ( -1.000000000000000000, 0.000000000000000000, 0.000000000000000000 ) ) ;
#15087 = ORIENTED_EDGE ( 'NONE', *, *, #16344, .T. ) ;
#15088 = CIRCLE ( 'NONE', #9093, 44.99999999999999289 ) ;
#15089 = CARTESIAN_POINT ( 'NONE',  ( 5.000000000000002665, -23.62010150527165919, -84.77081340225927875 ) ) ;
#15090 = AXIS2_PLACEMENT_3D ( 'NONE', #7646, #19038, #17813 ) ;
#15091 = CIRCLE ( 'NONE', #12267, 5.100000000000000533 ) ;
#15092 = FACE_OUTER_BOUND ( 'NONE', #2298, .T. ) ;
#15093 = AXIS2_PLACEMENT_3D ( 'NONE', #20924, #10870, #8002 ) ;
#15094 = EDGE_LOOP ( 'NONE', ( #7843, #12025, #14330, #19395 ) ) ;
#15095 = ORIENTED_EDGE ( 'NONE', *, *, #10313, .T. ) ;
#15096 = VERTEX_POINT ( 'NONE', #19432 ) ;
#15097 = ORIENTED_EDGE ( 'NONE', *, *, #13691, .F. ) ;
#15098 = CARTESIAN_POINT ( 'NONE',  ( 0.000000000000000000, -56.35896156214896280, -73.34918167666369015 ) ) ;
#15099 = ORIENTED_EDGE ( 'NONE', *, *, #7605, .F. ) ;
#15100 = CARTESIAN_POINT ( 'NONE',  ( 0.000000000000000000, -68.36541360927220978, 50.60987712331682076 ) ) ;
#15101 = CARTESIAN_POINT ( 'NONE',  ( 10.00000000000000000, 21.98203405400978383, -17.64965094506522192 ) ) ;
#15102 = DIRECTION ( 'NONE',  ( -1.000000000000000000, -0.000000000000000000, 0.000000000000000000 ) ) ;
#15103 = CARTESIAN_POINT ( 'NONE',  ( 10.00000000000000000, 74.74361964203228581, 40.60271866773572214 ) ) ;
#15104 = CYLINDRICAL_SURFACE ( 'NONE', #5072, 44.99999999999999289 ) ;
#15105 = AXIS2_PLACEMENT_3D ( 'NONE', #21111, #11158, #16011 ) ;
#15106 = EDGE_CURVE ( 'NONE', #6477, #17060, #8935, .T. ) ;
#15107 = CIRCLE ( 'NONE', #7722, 88.00000000000000000 ) ;
#15108 = DIRECTION ( 'NONE',  ( -1.000000000000000000, 0.000000000000000000, -0.000000000000000000 ) ) ;
#15109 = CARTESIAN_POINT ( 'NONE',  ( 10.00000000000000000, 0.000000000000000000, 0.000000000000000000 ) ) ;
#15110 = CIRCLE ( 'NONE', #12285, 27.49900000000000588 ) ;
#15111 = CIRCLE ( 'NONE', #998, 92.50100000000000477 ) ;
#15112 = CARTESIAN_POINT ( 'NONE',  ( 0.000000000000000000, 0.000000000000000000, 0.000000000000000000 ) ) ;
#15113 = DIRECTION ( 'NONE',  ( -1.000000000000000000, -0.000000000000000000, -0.000000000000000000 ) ) ;
#15114 = DIRECTION ( 'NONE',  ( 0.000000000000000000, 0.000000000000000000, -1.000000000000000000 ) ) ;
#15115 = ORIENTED_EDGE ( 'NONE', *, *, #10407, .F. ) ;
#15116 =( LENGTH_UNIT ( ) NAMED_UNIT ( * ) SI_UNIT ( .MILLI., .METRE. ) );
#15117 = VERTEX_POINT ( 'NONE', #17459 ) ;
#15118 = CARTESIAN_POINT ( 'NONE',  ( 10.00000000000000000, 81.55207211302078463, -24.17537951050094236 ) ) ;
#15119 = ORIENTED_EDGE ( 'NONE', *, *, #1093, .T. ) ;
#15120 = EDGE_CURVE ( 'NONE', #14060, #20435, #15845, .T. ) ;
#15121 = AXIS2_PLACEMENT_3D ( 'NONE', #5404, #18681, #13804 ) ;
#15122 = EDGE_LOOP ( 'NONE', ( #14738, #221, #11263, #6443, #19066, #21239 ) ) ;
#15123 = AXIS2_PLACEMENT_3D ( 'NONE', #3951, #20539, #532 ) ;
#15124 = AXIS2_PLACEMENT_3D ( 'NONE', #8782, #17397, #20715 ) ;
#15125 = EDGE_LOOP ( 'NONE', ( #13152, #13696, #115, #20488 ) ) ;
#15126 = ADVANCED_FACE ( 'NONE', ( #15792 ), #14463, .F. ) ;
#15127 = DIRECTION ( 'NONE',  ( -1.000000000000000000, 0.000000000000000000, 0.000000000000000000 ) ) ;
#15128 = VERTEX_POINT ( 'NONE', #20872 ) ;
#15129 = CARTESIAN_POINT ( 'NONE',  ( -90.00000000000000000, 0.000000000000000000, 0.000000000000000000 ) ) ;
#15130 = CARTESIAN_POINT ( 'NONE',  ( 5.000000000000002665, -11.59241532900687233, 87.23311244498734141 ) ) ;
#15131 = EDGE_CURVE ( 'NONE', #12455, #14957, #21492, .T. ) ;
#15132 = CARTESIAN_POINT ( 'NONE',  ( 10.00000000000000000, 3.728035544477412255, -84.97818067823766341 ) ) ;
#15133 = EDGE_CURVE ( 'NONE', #4328, #18178, #2423, .T. ) ;
#15134 = EDGE_CURVE ( 'NONE', #16786, #52, #19719, .T. ) ;
#15135 = CARTESIAN_POINT ( 'NONE',  ( 0.000000000000000000, -31.15801000616886896, 79.14775961996379294 ) ) ;
#15136 = FACE_OUTER_BOUND ( 'NONE', #3677, .T. ) ;
#15137 = CIRCLE ( 'NONE', #20789, 92.50100000000000477 ) ;
#15138 = ADVANCED_FACE ( 'NONE', ( #15903 ), #14024, .F. ) ;
#15139 = AXIS2_PLACEMENT_3D ( 'NONE', #2371, #12214, #17635 ) ;
#15140 = VERTEX_POINT ( 'NONE', #19327 ) ;
#15141 = CIRCLE ( 'NONE', #20795, 0.2042000000000016025 ) ;
#15142 = DIRECTION ( 'NONE',  ( 0.000000000000000000, 0.1391731009600591373, 0.9902680687415712502 ) ) ;
#15143 = ORIENTED_EDGE ( 'NONE', *, *, #2343, .T. ) ;
#15144 = ORIENTED_EDGE ( 'NONE', *, *, #21302, .F. ) ;
#15145 = ADVANCED_FACE ( 'NONE', ( #10926 ), #4293, .F. ) ;
#15146 = FACE_OUTER_BOUND ( 'NONE', #17678, .T. ) ;
#15147 = EDGE_LOOP ( 'NONE', ( #5621, #1021, #20696, #15196 ) ) ;
#15148 = CARTESIAN_POINT ( 'NONE',  ( 10.00000000000000000, -61.33825423015729683, 69.23910433415923649 ) ) ;
#15149 = VERTEX_POINT ( 'NONE', #15005 ) ;
#15150 = VERTEX_POINT ( 'NONE', #21634 ) ;
#15151 = ADVANCED_FACE ( 'NONE', ( #16233, #11149 ), #14565, .T. ) ;
#15152 = CIRCLE ( 'NONE', #11277, 88.00000000000000000 ) ;
#15153 = DIRECTION ( 'NONE',  ( -1.000000000000000000, 0.000000000000000000, 0.000000000000000000 ) ) ;
#15154 = ORIENTED_EDGE ( 'NONE', *, *, #19852, .T. ) ;
#15155 = AXIS2_PLACEMENT_3D ( 'NONE', #475, #693, #2132 ) ;
#15156 = VECTOR ( 'NONE', #416, 1000.000000000000000 ) ;
#15157 = DIRECTION ( 'NONE',  ( 0.000000000000000000, 0.000000000000000000, 1.000000000000000000 ) ) ;
#15158 = EDGE_CURVE ( 'NONE', #20507, #12373, #6685, .T. ) ;
#15159 = CYLINDRICAL_SURFACE ( 'NONE', #2647, 92.50100000000000477 ) ;
#15160 = FACE_OUTER_BOUND ( 'NONE', #17540, .T. ) ;
#15161 = FACE_OUTER_BOUND ( 'NONE', #20585, .T. ) ;
#15162 = FACE_OUTER_BOUND ( 'NONE', #19779, .T. ) ;
#15163 = DIRECTION ( 'NONE',  ( 1.000000000000000000, 0.000000000000000000, 0.000000000000000000 ) ) ;
#15164 = DIRECTION ( 'NONE',  ( -1.000000000000000000, 0.000000000000000000, 0.000000000000000000 ) ) ;
#15165 = EDGE_CURVE ( 'NONE', #14214, #21189, #17616, .T. ) ;
#15166 = VERTEX_POINT ( 'NONE', #18341 ) ;
#15167 = EDGE_CURVE ( 'NONE', #7466, #15171, #4848, .T. ) ;
#15168 = VECTOR ( 'NONE', #17050, 1000.000000000000000 ) ;
#15169 = DIRECTION ( 'NONE',  ( 0.000000000000000000, 0.000000000000000000, 1.000000000000000000 ) ) ;
#15170 = DIRECTION ( 'NONE',  ( 0.000000000000000000, 0.2079116908177532363, 0.9781476007338069101 ) ) ;
#15171 = VERTEX_POINT ( 'NONE', #11359 ) ;
#15172 = CARTESIAN_POINT ( 'NONE',  ( 1.200000000000006617, 0.000000000000000000, 0.000000000000000000 ) ) ;
#15173 = EDGE_CURVE ( 'NONE', #14408, #6716, #19017, .T. ) ;
#15174 = VERTEX_POINT ( 'NONE', #11475 ) ;
#15175 =( LENGTH_UNIT ( ) NAMED_UNIT ( * ) SI_UNIT ( .MILLI., .METRE. ) );
#15176 = ORIENTED_EDGE ( 'NONE', *, *, #12846, .T. ) ;
#15177 = DIRECTION ( 'NONE',  ( -1.000000000000000000, -0.000000000000000000, -0.000000000000000000 ) ) ;
#15178 = ORIENTED_EDGE ( 'NONE', *, *, #182, .T. ) ;
#15179 = ORIENTED_EDGE ( 'NONE', *, *, #15946, .T. ) ;
#15180 = DIRECTION ( 'NONE',  ( 0.000000000000000000, 0.000000000000000000, 1.000000000000000000 ) ) ;
#15181 = DIRECTION ( 'NONE',  ( 0.000000000000000000, 0.1391731009600591928, 0.9902680687415711391 ) ) ;
#15182 = ORIENTED_EDGE ( 'NONE', *, *, #10575, .T. ) ;
#15183 = EDGE_CURVE ( 'NONE', #1127, #11594, #12662, .T. ) ;
#15184 = DIRECTION ( 'NONE',  ( -1.000000000000000000, 0.000000000000000000, 0.000000000000000000 ) ) ;
#15185 = DIRECTION ( 'NONE',  ( 0.000000000000000000, 0.000000000000000000, 1.000000000000000000 ) ) ;
#15186 = CARTESIAN_POINT ( 'NONE',  ( 10.00000000000000000, -19.29292659244022445, 25.53004080487755445 ) ) ;
#15187 = VECTOR ( 'NONE', #6289, 1000.000000000000000 ) ;
#15188 = DIRECTION ( 'NONE',  ( 1.000000000000000000, 0.000000000000000000, 0.000000000000000000 ) ) ;
#15189 = CARTESIAN_POINT ( 'NONE',  ( 0.000000000000000000, -23.10190250628774322, -89.56973317806621537 ) ) ;
#15190 = CARTESIAN_POINT ( 'NONE',  ( 10.00000000000000000, 46.07110168784820559, 74.97635353408399794 ) ) ;
#15191 = VERTEX_POINT ( 'NONE', #3079 ) ;
#15192 = DIRECTION ( 'NONE',  ( 1.000000000000000000, -0.000000000000000000, -0.000000000000000000 ) ) ;
#15193 = CARTESIAN_POINT ( 'NONE',  ( 150.0000507999999968, 0.000000000000000000, 0.000000000000000000 ) ) ;
#15194 = ORIENTED_EDGE ( 'NONE', *, *, #18800, .T. ) ;
#15195 = CYLINDRICAL_SURFACE ( 'NONE', #9429, 92.50100000000000477 ) ;
#15196 = ORIENTED_EDGE ( 'NONE', *, *, #6086, .F. ) ;
#15197 = PRESENTATION_STYLE_ASSIGNMENT (( #5043 ) ) ;
#15198 = CIRCLE ( 'NONE', #1787, 12.00000000000000000 ) ;
#15199 = CARTESIAN_POINT ( 'NONE',  ( 0.000000000000000000, -78.83848282823942100, 48.38314403117473006 ) ) ;
#15200 = ADVANCED_FACE ( 'NONE', ( #19656 ), #13123, .F. ) ;
#15201 = ORIENTED_EDGE ( 'NONE', *, *, #16107, .F. ) ;
#15202 = FACE_OUTER_BOUND ( 'NONE', #8303, .T. ) ;
#15203 = EDGE_LOOP ( 'NONE', ( #1171, #16549, #18916, #21380 ) ) ;
#15204 = EDGE_LOOP ( 'NONE', ( #13550, #2323, #124, #5673 ) ) ;
#15205 = VERTEX_POINT ( 'NONE', #17898 ) ;
#15206 = CARTESIAN_POINT ( 'NONE',  ( -7.600000000000002309, 0.000000000000000000, -114.9007999999999896 ) ) ;
#15207 = ORIENTED_EDGE ( 'NONE', *, *, #11483, .F. ) ;
#15208 = CARTESIAN_POINT ( 'NONE',  ( 10.00000000000000000, -57.53593069156421791, 72.42963261300944566 ) ) ;
#15209 = DIRECTION ( 'NONE',  ( 0.000000000000000000, 0.000000000000000000, -1.000000000000000000 ) ) ;
#15210 = DIRECTION ( 'NONE',  ( 1.000000000000000000, 0.000000000000000000, 0.000000000000000000 ) ) ;
#15211 = DIRECTION ( 'NONE',  ( 0.000000000000000000, 0.000000000000000000, -1.000000000000000000 ) ) ;
#15212 = CARTESIAN_POINT ( 'NONE',  ( 10.00000000000000000, -21.31452625070983231, 82.34610137166113475 ) ) ;
#15213 = CARTESIAN_POINT ( 'NONE',  ( 10.00000000000000000, 0.000000000000000000, 0.000000000000000000 ) ) ;
#15214 = DIRECTION ( 'NONE',  ( 0.000000000000000000, 0.2756373558169998295, -0.9612616959383187831 ) ) ;
#15215 = DIRECTION ( 'NONE',  ( -1.000000000000000000, -0.000000000000000000, -0.000000000000000000 ) ) ;
#15216 = DIRECTION ( 'NONE',  ( 0.000000000000000000, 0.000000000000000000, 1.000000000000000000 ) ) ;
#15217 = CARTESIAN_POINT ( 'NONE',  ( 1.500000000000001332, 0.000000000000000000, 0.000000000000000000 ) ) ;
#15218 = ORIENTED_EDGE ( 'NONE', *, *, #20504, .T. ) ;
#15219 = CARTESIAN_POINT ( 'NONE',  ( 0.000000000000000000, 92.32475887865433606, -5.707354816229567973 ) ) ;
#15220 = ORIENTED_EDGE ( 'NONE', *, *, #11376, .T. ) ;
#15221 = LINE ( 'NONE', #6105, #5608 ) ;
#15222 = ORIENTED_EDGE ( 'NONE', *, *, #21523, .F. ) ;
#15223 = ORIENTED_EDGE ( 'NONE', *, *, #6689, .F. ) ;
#15224 = ADVANCED_FACE ( 'NONE', ( #7830 ), #21307, .F. ) ;
#15225 = AXIS2_PLACEMENT_3D ( 'NONE', #15880, #2172, #15645 ) ;
#15226 = ORIENTED_EDGE ( 'NONE', *, *, #16027, .T. ) ;
#15227 = CARTESIAN_POINT ( 'NONE',  ( 0.000000000000000000, -79.66702613806795341, 29.80527447819410369 ) ) ;
#15228 = ORIENTED_EDGE ( 'NONE', *, *, #2748, .F. ) ;
#15229 = CARTESIAN_POINT ( 'NONE',  ( 0.000000000000000000, 86.77540292929722909, -14.62974526292624944 ) ) ;
#15230 = DIRECTION ( 'NONE',  ( 0.000000000000000000, -0.7431448254773862505, -0.6691306063588668973 ) ) ;
#15231 = EDGE_CURVE ( 'NONE', #9187, #7466, #7034, .T. ) ;
#15232 = AXIS2_PLACEMENT_3D ( 'NONE', #16656, #15102, #5174 ) ;
#15233 = CARTESIAN_POINT ( 'NONE',  ( 10.00000000000000000, 21.69483248597422076, 16.89761061231787309 ) ) ;
#15234 = CARTESIAN_POINT ( 'NONE',  ( 10.00000000000000000, -67.05625154133495869, 63.71729851637790176 ) ) ;
#15235 = DIRECTION ( 'NONE',  ( 0.000000000000000000, 0.9945218953682736229, -0.1045284632676503761 ) ) ;
#15236 = CARTESIAN_POINT ( 'NONE',  ( 0.000000000000000000, -22.77465461094683974, 15.41136296218079238 ) ) ;
#15237 = EDGE_CURVE ( 'NONE', #7417, #14214, #4732, .T. ) ;
#15238 = DIRECTION ( 'NONE',  ( -1.000000000000000000, 0.000000000000000000, 0.000000000000000000 ) ) ;
#15239 = VERTEX_POINT ( 'NONE', #2862 ) ;
#15240 = DIRECTION ( 'NONE',  ( 0.000000000000000000, 0.4067366430757948237, 0.9135454576426033091 ) ) ;
#15241 = AXIS2_PLACEMENT_3D ( 'NONE', #2873, #9381, #12596 ) ;
#15242 = ORIENTED_EDGE ( 'NONE', *, *, #2584, .T. ) ;
#15243 = ORIENTED_EDGE ( 'NONE', *, *, #9411, .T. ) ;
#15244 = CARTESIAN_POINT ( 'NONE',  ( 123.5000000000000142, 0.000000000000000000, 25.00000000000000000 ) ) ;
#15245 = CIRCLE ( 'NONE', #14898, 88.00000000000000000 ) ;
#15246 = ORIENTED_EDGE ( 'NONE', *, *, #11092, .F. ) ;
#15247 = EDGE_CURVE ( 'NONE', #7775, #3621, #17982, .T. ) ;
#15248 = EDGE_CURVE ( 'NONE', #8096, #20717, #1032, .T. ) ;
#15249 = CARTESIAN_POINT ( 'NONE',  ( 10.00000000000000000, 14.02138820414913845, 83.89630571862289798 ) ) ;
#15250 = ORIENTED_EDGE ( 'NONE', *, *, #2325, .F. ) ;
#15251 = ORIENTED_EDGE ( 'NONE', *, *, #10117, .T. ) ;
#15252 = APPLICATION_PROTOCOL_DEFINITION ( 'draft international standard', 'automotive_design', 1998, #14469 ) ;
#15253 = AXIS2_PLACEMENT_3D ( 'NONE', #3515, #19985, #11588 ) ;
#15254 = LINE ( 'NONE', #11632, #21105 ) ;
#15255 = EDGE_CURVE ( 'NONE', #10982, #21052, #16922, .T. ) ;
#15256 = ORIENTED_EDGE ( 'NONE', *, *, #15867, .F. ) ;
#15257 = CYLINDRICAL_SURFACE ( 'NONE', #3869, 44.99999999999999289 ) ;
#15258 = AXIS2_PLACEMENT_3D ( 'NONE', #5409, #15463, #19106 ) ;
#15259 = CARTESIAN_POINT ( 'NONE',  ( 0.000000000000000000, 37.96946988134275358, -76.11510229470822253 ) ) ;
#15260 = DIRECTION ( 'NONE',  ( -1.000000000000000000, -0.000000000000000000, -0.000000000000000000 ) ) ;
#15261 = CARTESIAN_POINT ( 'NONE',  ( -10.49999999999999822, 0.000000000000000000, 3.000000000000000000 ) ) ;
#15262 = FACE_BOUND ( 'NONE', #8091, .T. ) ;
#15263 = CYLINDRICAL_SURFACE ( 'NONE', #16435, 27.49900000000000233 ) ;
#15264 = ADVANCED_FACE ( 'NONE', ( #1316 ), #2964, .F. ) ;
#15265 = DIRECTION ( 'NONE',  ( -1.000000000000000000, -0.000000000000000000, 0.000000000000000000 ) ) ;
#15266 = AXIS2_PLACEMENT_3D ( 'NONE', #548, #10808, #5520 ) ;
#15267 = CIRCLE ( 'NONE', #7859, 32.00000000000000000 ) ;
#15268 = ORIENTED_EDGE ( 'NONE', *, *, #18247, .T. ) ;
#15269 = CIRCLE ( 'NONE', #7514, 88.00000000000000000 ) ;
#15270 = EDGE_CURVE ( 'NONE', #16155, #21814, #1048, .T. ) ;
#15271 = LINE ( 'NONE', #15601, #9801 ) ;
#15272 = CARTESIAN_POINT ( 'NONE',  ( 10.00000000000000000, 12.94633825542266869, 24.26081875733338933 ) ) ;
#15273 = VERTEX_POINT ( 'NONE', #8168 ) ;
#15274 = CARTESIAN_POINT ( 'NONE',  ( 0.000000000000000000, 57.47876254627226444, -62.70072803846332476 ) ) ;
#15275 = VERTEX_POINT ( 'NONE', #14897 ) ;
#15276 = ORIENTED_EDGE ( 'NONE', *, *, #10591, .T. ) ;
#15277 = AXIS2_PLACEMENT_3D ( 'NONE', #17183, #3808, #61 ) ;
#15279 = CIRCLE ( 'NONE', #18120, 45.00000000000000711 ) ;
#15278 = DIRECTION ( 'NONE',  ( 1.000000000000000000, 0.000000000000000000, 0.000000000000000000 ) ) ;
#15280 = ADVANCED_FACE ( 'NONE', ( #20529 ), #10023, .F. ) ;
#15281 = EDGE_LOOP ( 'NONE', ( #11860, #8601, #20023, #5199 ) ) ;
#15282 = ORIENTED_EDGE ( 'NONE', *, *, #6197, .F. ) ;
#15283 = DIRECTION ( 'NONE',  ( 1.000000000000000000, -0.000000000000000000, -0.000000000000000000 ) ) ;
#15284 = LINE ( 'NONE', #268, #12768 ) ;
#15285 = AXIS2_PLACEMENT_3D ( 'NONE', #1628, #78, #10127 ) ;
#15286 = VERTEX_POINT ( 'NONE', #6740 ) ;
#15287 = CARTESIAN_POINT ( 'NONE',  ( 5.000000000000000000, -52.25832601289145884, 70.80301803122767978 ) ) ;
#15288 = CARTESIAN_POINT ( 'NONE',  ( -140.0000507999999968, 3.673940397442060361E-16, -3.000000000000000444 ) ) ;
#15289 = CARTESIAN_POINT ( 'NONE',  ( 10.00000000000000000, 0.000000000000000000, 0.000000000000000000 ) ) ;
#15290 = LINE ( 'NONE', #13968, #1201 ) ;
#15291 = CYLINDRICAL_SURFACE ( 'NONE', #11754, 88.00000000000000000 ) ;
#15292 = FACE_OUTER_BOUND ( 'NONE', #17467, .T. ) ;
#15293 = EDGE_CURVE ( 'NONE', #5244, #12424, #10207, .T. ) ;
#15294 = AXIS2_PLACEMENT_3D ( 'NONE', #21278, #15761, #6155 ) ;
#15295 = ORIENTED_EDGE ( 'NONE', *, *, #8030, .F. ) ;
#15296 = ADVANCED_FACE ( 'NONE', ( #318 ), #12121, .F. ) ;
#15297 = CARTESIAN_POINT ( 'NONE',  ( 0.000000000000000000, 69.25892805976512534, 49.38005998797868301 ) ) ;
#15298 = AXIS2_PLACEMENT_3D ( 'NONE', #14175, #16276, #19597 ) ;
#15299 = DIRECTION ( 'NONE',  ( 0.000000000000000000, 0.000000000000000000, -1.000000000000000000 ) ) ;
#15300 = ORIENTED_EDGE ( 'NONE', *, *, #2755, .T. ) ;
#15301 = EDGE_CURVE ( 'NONE', #17030, #393, #2449, .T. ) ;
#15302 = AXIS2_PLACEMENT_3D ( 'NONE', #16728, #15283, #20056 ) ;
#15303 = EDGE_CURVE ( 'NONE', #8003, #3473, #7061, .T. ) ;
#15304 = DIRECTION ( 'NONE',  ( 0.000000000000000000, 0.000000000000000000, -1.000000000000000000 ) ) ;
#15305 = VERTEX_POINT ( 'NONE', #88 ) ;
#15306 = FACE_OUTER_BOUND ( 'NONE', #11428, .T. ) ;
#15307 = CARTESIAN_POINT ( 'NONE',  ( 10.00000000000000000, 0.000000000000000000, 0.000000000000000000 ) ) ;
#15308 = ORIENTED_EDGE ( 'NONE', *, *, #2162, .T. ) ;
#15309 = ORIENTED_EDGE ( 'NONE', *, *, #3911, .T. ) ;
#15310 = VERTEX_POINT ( 'NONE', #18552 ) ;
#15311 = EDGE_LOOP ( 'NONE', ( #8952, #19518, #11156, #9053 ) ) ;
#15312 = DIRECTION ( 'NONE',  ( 0.000000000000000000, -8.866364432770349300E-15, -1.000000000000000000 ) ) ;
#15313 = ORIENTED_EDGE ( 'NONE', *, *, #8700, .F. ) ;
#15314 = DIRECTION ( 'NONE',  ( 0.000000000000000000, 0.000000000000000000, 1.000000000000000000 ) ) ;
#15315 = VECTOR ( 'NONE', #623, 1000.000000000000000 ) ;
#15316 = DIRECTION ( 'NONE',  ( -1.000000000000000000, -0.000000000000000000, 0.000000000000000000 ) ) ;
#15317 = DIRECTION ( 'NONE',  ( 1.000000000000000000, 0.000000000000000000, 0.000000000000000000 ) ) ;
#15318 = DIRECTION ( 'NONE',  ( 0.000000000000000000, 0.000000000000000000, 1.000000000000000000 ) ) ;
#15319 = PRODUCT_DEFINITION_SHAPE ( 'NONE', 'NONE',  #3340 ) ;
#15320 = AXIS2_PLACEMENT_3D ( 'NONE', #14394, #2801, #2681 ) ;
#15321 = CARTESIAN_POINT ( 'NONE',  ( 10.00000000000000000, 33.95793648385932784, -86.04239391577952745 ) ) ;
#15322 = CARTESIAN_POINT ( 'NONE',  ( 0.000000000000000000, -83.03980459022491800, 18.42770452393216374 ) ) ;
#15323 = DIRECTION ( 'NONE',  ( -1.000000000000000000, -0.000000000000000000, -0.000000000000000000 ) ) ;
#15324 = CARTESIAN_POINT ( 'NONE',  ( 10.00000000000000000, -61.71252885873347793, -58.53847642588656441 ) ) ;
#15325 = AXIS2_PLACEMENT_3D ( 'NONE', #17456, #15789, #8932 ) ;
#15326 = CARTESIAN_POINT ( 'NONE',  ( 5.000000000000002665, 29.47587714451147534, -82.91666097089093057 ) ) ;
#15327 = AXIS2_PLACEMENT_3D ( 'NONE', #4140, #14182, #17302 ) ;
#15328 = CARTESIAN_POINT ( 'NONE',  ( 0.000000000000000000, -12.90135963484022241, -87.04915231966658951 ) ) ;
#15329 = ORIENTED_EDGE ( 'NONE', *, *, #3262, .T. ) ;
#15330 = CARTESIAN_POINT ( 'NONE',  ( 5.000000000000000000, 67.00000000000000000, 9.999999999999998224 ) ) ;
#15331 = ORIENTED_EDGE ( 'NONE', *, *, #12288, .F. ) ;
#15332 = FACE_OUTER_BOUND ( 'NONE', #13883, .T. ) ;
#15333 = VECTOR ( 'NONE', #12459, 1000.000000000000000 ) ;
#15334 = VERTEX_POINT ( 'NONE', #18763 ) ;
#15335 = ORIENTED_EDGE ( 'NONE', *, *, #1052, .F. ) ;
#15336 = ORIENTED_EDGE ( 'NONE', *, *, #19145, .F. ) ;
#15337 = FACE_OUTER_BOUND ( 'NONE', #7388, .T. ) ;
#15338 = AXIS2_PLACEMENT_3D ( 'NONE', #19213, #9153, #15900 ) ;
#15339 = ORIENTED_EDGE ( 'NONE', *, *, #14344, .T. ) ;
#15340 = DIRECTION ( 'NONE',  ( 1.000000000000000000, 0.000000000000000000, 0.000000000000000000 ) ) ;
#15341 = CIRCLE ( 'NONE', #17809, 123.5000000000000142 ) ;
#15342 = SURFACE_STYLE_USAGE ( .BOTH. , #2194 ) ;
#15343 = AXIS2_PLACEMENT_3D ( 'NONE', #11112, #7474, #21174 ) ;
#15344 = AXIS2_PLACEMENT_3D ( 'NONE', #6453, #11079, #11407 ) ;
#15345 = CARTESIAN_POINT ( 'NONE',  ( 10.00000000000000000, -90.32141448704669529, -19.96189084378313794 ) ) ;
#15346 = DIRECTION ( 'NONE',  ( 1.000000000000000000, 0.000000000000000000, 0.000000000000000000 ) ) ;
#15347 = CARTESIAN_POINT ( 'NONE',  ( 10.00000000000000000, 0.000000000000000000, 0.000000000000000000 ) ) ;
#15348 = CIRCLE ( 'NONE', #2652, 92.50100000000000477 ) ;
#15349 = DIRECTION ( 'NONE',  ( -1.000000000000000000, -0.000000000000000000, -0.000000000000000000 ) ) ;
#15350 = DIRECTION ( 'NONE',  ( -1.000000000000000000, 0.000000000000000000, -0.000000000000000000 ) ) ;
#15351 = EDGE_CURVE ( 'NONE', #4335, #7874, #1404, .T. ) ;
#15352 = CLOSED_SHELL ( 'NONE', ( #19446, #19475, #13254, #5974, #10657, #3237, #3799, #16797, #5868, #9821, #4984, #19568, #810, #1069, #6421, #10027, #19045, #17347, #4220, #8918, #11038, #17146, #17892, #2551, #696, #18392, #17984, #3289, #2047, #16257, #7262, #5112, #719, #15681, #7978, #14584, #15014, #1938, #3922, #8226, #1326, #6708, #2118, #3519, #3113, #14230, #7090, #5597, #7730, #11059, #5311, #12433, #4996, #21074, #793, #4107, #8014, #2073, #9329, #18123, #16890, #8262, #5539, #4842, #5048, #13490, #20701, #8758, #15832, #11644, #15736, #7433, #14578, #5688, #2289, #16300, #5586, #10820, #2833, #18566, #20713, #18646, #13690, #4920, #10304, #3658, #1619, #20255, #10544, #18640, #17433, #16239, #16585, #20668, #2164, #12549, #19430, #5299, #7809, #13963, #11930, #11851, #16608, #17048, #13911, #175, #4477, #19190, #15379, #9868, #2202, #18967, #14724, #5412, #13610, #18518, #18272, #7687, #18017, #8621, #11647, #21332, #17330, #5420, #21480, #11883, #8541, #18459, #10516, #17894, #17295, #19495, #671, #21784, #16933, #20783 ) ) ;
#15353 = ORIENTED_EDGE ( 'NONE', *, *, #20131, .T. ) ;
#15354 = CARTESIAN_POINT ( 'NONE',  ( 10.00000000000000000, -15.25521607131222268, 23.70650506194164464 ) ) ;
#15355 = CIRCLE ( 'NONE', #17829, 88.00000000000000000 ) ;
#15356 = ORIENTED_EDGE ( 'NONE', *, *, #10270, .T. ) ;
#15357 = VECTOR ( 'NONE', #4121, 1000.000000000000000 ) ;
#15358 = EDGE_CURVE ( 'NONE', #10039, #16416, #13376, .T. ) ;
#15359 = AXIS2_PLACEMENT_3D ( 'NONE', #8461, #18838, #16965 ) ;
#15360 = ORIENTED_EDGE ( 'NONE', *, *, #936, .F. ) ;
#15361 = AXIS2_PLACEMENT_3D ( 'NONE', #19346, #7521, #10945 ) ;
#15362 = CARTESIAN_POINT ( 'NONE',  ( 10.00000000000000000, -23.62010150527279961, 84.77081340225898032 ) ) ;
#15363 = ORIENTED_EDGE ( 'NONE', *, *, #16344, .F. ) ;
#15364 = EDGE_LOOP ( 'NONE', ( #12242, #16316, #21268, #8892 ) ) ;
#15365 = CARTESIAN_POINT ( 'NONE',  ( 5.000000000000000888, -31.88200538760795766, 2.745493118646880504 ) ) ;
#15366 = ORIENTED_EDGE ( 'NONE', *, *, #13286, .F. ) ;
#15367 = CARTESIAN_POINT ( 'NONE',  ( 9.999999999999980460, 0.000000000000000000, -113.8250000000000171 ) ) ;
#15368 = CARTESIAN_POINT ( 'NONE',  ( 10.00000000000000000, 83.48638250753266732, -27.82128566055030916 ) ) ;
#15369 = DIRECTION ( 'NONE',  ( 0.000000000000000000, 0.000000000000000000, 1.000000000000000000 ) ) ;
#15370 = VECTOR ( 'NONE', #7431, 1000.000000000000000 ) ;
#15371 = CARTESIAN_POINT ( 'NONE',  ( 7.599999999999998757, 0.000000000000000000, 0.000000000000000000 ) ) ;
#15372 = AXIS2_PLACEMENT_3D ( 'NONE', #7557, #2480, #9206 ) ;
#15373 = AXIS2_PLACEMENT_3D ( 'NONE', #5113, #5440, #363 ) ;
#15374 = DIRECTION ( 'NONE',  ( 1.000000000000000000, 0.000000000000000000, 0.000000000000000000 ) ) ;
#15375 = DIRECTION ( 'NONE',  ( 0.000000000000000000, 0.000000000000000000, 1.000000000000000000 ) ) ;
#15377 = VECTOR ( 'NONE', #10913, 1000.000000000000000 ) ;
#15376 = FACE_OUTER_BOUND ( 'NONE', #5980, .T. ) ;
#15378 = ADVANCED_FACE ( 'NONE', ( #210 ), #3732, .F. ) ;
#15379 = ADVANCED_FACE ( 'NONE', ( #3616 ), #5068, .T. ) ;
#15380 = VERTEX_POINT ( 'NONE', #20202 ) ;
#15381 = DIRECTION ( 'NONE',  ( 0.000000000000000000, 0.000000000000000000, 1.000000000000000000 ) ) ;
#15382 = CARTESIAN_POINT ( 'NONE',  ( 0.000000000000000000, 0.000000000000000000, 0.000000000000000000 ) ) ;
#15383 = ORIENTED_EDGE ( 'NONE', *, *, #2440, .F. ) ;
#15384 = CIRCLE ( 'NONE', #15031, 45.00000000000000711 ) ;
#15385 = DIRECTION ( 'NONE',  ( -1.000000000000000000, -0.000000000000000000, 0.000000000000000000 ) ) ;
#15386 = ORIENTED_EDGE ( 'NONE', *, *, #8900, .F. ) ;
#15387 = SURFACE_SIDE_STYLE ('',( #18400 ) ) ;
#15388 = AXIS2_PLACEMENT_3D ( 'NONE', #18756, #20523, #17213 ) ;
#15389 = EDGE_CURVE ( 'NONE', #8475, #20752, #3164, .T. ) ;
#15390 = ORIENTED_EDGE ( 'NONE', *, *, #7215, .F. ) ;
#15391 = DIRECTION ( 'NONE',  ( -1.000000000000000000, -0.000000000000000000, -0.000000000000000000 ) ) ;
#15392 = ORIENTED_EDGE ( 'NONE', *, *, #14705, .F. ) ;
#15393 = ORIENTED_EDGE ( 'NONE', *, *, #3556, .F. ) ;
#15394 = CARTESIAN_POINT ( 'NONE',  ( 6.123233995736766282E-16, 100.0000000000000000, 5.000000000000000000 ) ) ;
#15395 = DIRECTION ( 'NONE',  ( -1.000000000000000000, -0.000000000000000000, -0.000000000000000000 ) ) ;
#15396 = ADVANCED_FACE ( 'NONE', ( #11803 ), #8815, .F. ) ;
#15397 = DIRECTION ( 'NONE',  ( -1.000000000000000000, -0.000000000000000000, -0.000000000000000000 ) ) ;
#15398 = CARTESIAN_POINT ( 'NONE',  ( 1.114299999999999846, 0.000000000000000000, 0.000000000000000000 ) ) ;
#15399 = DIRECTION ( 'NONE',  ( 0.000000000000000000, 1.773272886554069860E-14, -1.000000000000000000 ) ) ;
#15400 = DIRECTION ( 'NONE',  ( -1.000000000000000000, 0.000000000000000000, 0.000000000000000000 ) ) ;
#15401 = DIRECTION ( 'NONE',  ( 0.000000000000000000, -1.063963731932441790E-14, -1.000000000000000000 ) ) ;
#15402 = DIRECTION ( 'NONE',  ( 0.000000000000000000, -0.5299192642331943537, -0.8480480961564326181 ) ) ;
#15403 = CIRCLE ( 'NONE', #8714, 88.00000000000000000 ) ;
#15404 = ADVANCED_FACE ( 'NONE', ( #4961 ), #10138, .F. ) ;
#15405 = CIRCLE ( 'NONE', #2006, 11.99999999999999822 ) ;
#15406 = CIRCLE ( 'NONE', #17188, 45.00000000000000000 ) ;
#15407 = EDGE_CURVE ( 'NONE', #6576, #19966, #8103, .T. ) ;
#15408 = ORIENTED_EDGE ( 'NONE', *, *, #21481, .F. ) ;
#15409 = AXIS2_PLACEMENT_3D ( 'NONE', #18361, #4649, #21325 ) ;
#15410 = LINE ( 'NONE', #17074, #3180 ) ;
#15411 = EDGE_CURVE ( 'NONE', #13148, #8199, #14452, .T. ) ;
#15412 = DIRECTION ( 'NONE',  ( 1.000000000000000000, 0.000000000000000000, -0.000000000000000000 ) ) ;
#15413 = EDGE_LOOP ( 'NONE', ( #12982, #4034, #1831, #236 ) ) ;
#15414 = CARTESIAN_POINT ( 'NONE',  ( 10.00000000000000000, 74.39348546125053474, 54.97312363261438151 ) ) ;
#15415 = ORIENTED_EDGE ( 'NONE', *, *, #10807, .F. ) ;
#15416 = FACE_OUTER_BOUND ( 'NONE', #11546, .T. ) ;
#15417 = CYLINDRICAL_SURFACE ( 'NONE', #8433, 88.00000000000000000 ) ;
#15418 = VERTEX_POINT ( 'NONE', #8593 ) ;
#15419 = CARTESIAN_POINT ( 'NONE',  ( 10.00000000000000000, -84.19736439813780748, -38.30455363801015523 ) ) ;
#15420 = EDGE_CURVE ( 'NONE', #20207, #13148, #8710, .T. ) ;
#15421 = AXIS2_PLACEMENT_3D ( 'NONE', #19008, #20225, #5089 ) ;
#15422 = ORIENTED_EDGE ( 'NONE', *, *, #15134, .F. ) ;
#15423 = ORIENTED_EDGE ( 'NONE', *, *, #11671, .F. ) ;
#15424 = CIRCLE ( 'NONE', #14004, 92.50100000000000477 ) ;
#15425 = ORIENTED_EDGE ( 'NONE', *, *, #8241, .T. ) ;
#15426 = DIRECTION ( 'NONE',  ( 1.000000000000000000, -0.000000000000000000, -0.000000000000000000 ) ) ;
#15427 = EDGE_CURVE ( 'NONE', #7563, #14716, #2110, .T. ) ;
#15428 = AXIS2_PLACEMENT_3D ( 'NONE', #12686, #2419, #19006 ) ;
#15429 = ORIENTED_EDGE ( 'NONE', *, *, #8001, .F. ) ;
#15430 = CARTESIAN_POINT ( 'NONE',  ( 10.00000000000000000, -78.83848282823942100, 48.38314403117473006 ) ) ;
#15431 = DIRECTION ( 'NONE',  ( 1.000000000000000000, 0.000000000000000000, 0.000000000000000000 ) ) ;
#15432 = FACE_OUTER_BOUND ( 'NONE', #4613, .T. ) ;
#15433 = DIRECTION ( 'NONE',  ( -1.000000000000000000, -0.000000000000000000, -0.000000000000000000 ) ) ;
#15434 = DIRECTION ( 'NONE',  ( 0.000000000000000000, -1.000000000000000000, 0.000000000000000000 ) ) ;
#15435 = EDGE_CURVE ( 'NONE', #21564, #17607, #19032, .T. ) ;
#15436 = CYLINDRICAL_SURFACE ( 'NONE', #14342, 27.49900000000000233 ) ;
#15437 = DIRECTION ( 'NONE',  ( 0.000000000000000000, 0.000000000000000000, 1.000000000000000000 ) ) ;
#15438 = DIRECTION ( 'NONE',  ( 0.000000000000000000, 0.000000000000000000, 1.000000000000000000 ) ) ;
#15439 = ORIENTED_EDGE ( 'NONE', *, *, #8749, .F. ) ;
#15440 = CARTESIAN_POINT ( 'NONE',  ( 5.000000000000000000, -72.58367602204151581, -49.75550195834942002 ) ) ;
#15441 = AXIS2_PLACEMENT_3D ( 'NONE', #21097, #657, #983 ) ;
#15442 = EDGE_CURVE ( 'NONE', #12701, #15128, #17326, .T. ) ;
#15443 = CARTESIAN_POINT ( 'NONE',  ( 10.00000000000000000, 72.58367602204188529, 49.75550195834890843 ) ) ;
#15444 = AXIS2_PLACEMENT_3D ( 'NONE', #6606, #20078, #3382 ) ;
#15445 = FACE_OUTER_BOUND ( 'NONE', #14123, .T. ) ;
#15446 = ORIENTED_EDGE ( 'NONE', *, *, #18671, .T. ) ;
#15447 = LINE ( 'NONE', #5073, #17596 ) ;
#15448 = VERTEX_POINT ( 'NONE', #19409 ) ;
#15449 = LINE ( 'NONE', #325, #8069 ) ;
#15450 = ORIENTED_EDGE ( 'NONE', *, *, #1503, .T. ) ;
#15451 = CIRCLE ( 'NONE', #5931, 7.500000000000000000 ) ;
#15452 = ORIENTED_EDGE ( 'NONE', *, *, #17851, .F. ) ;
#15453 = VERTEX_POINT ( 'NONE', #21067 ) ;
#15454 = CARTESIAN_POINT ( 'NONE',  ( 0.000000000000000000, 26.27606311335965827, -10.21217444509384364 ) ) ;
#15455 = VECTOR ( 'NONE', #10774, 1000.000000000000000 ) ;
#15456 = CIRCLE ( 'NONE', #18998, 44.99999999999999289 ) ;
#15457 = ORIENTED_EDGE ( 'NONE', *, *, #5196, .T. ) ;
#15458 = DIRECTION ( 'NONE',  ( 0.000000000000000000, -0.4067366430757888285, -0.9135454576426059736 ) ) ;
#15459 = CARTESIAN_POINT ( 'NONE',  ( 0.000000000000000000, 0.000000000000000000, -5.000000000000000000 ) ) ;
#15460 = AXIS2_PLACEMENT_3D ( 'NONE', #8861, #12181, #13507 ) ;
#15461 = AXIS2_PLACEMENT_3D ( 'NONE', #9332, #17645, #12873 ) ;
#15462 = CIRCLE ( 'NONE', #5576, 88.00000000000000000 ) ;
#15463 = DIRECTION ( 'NONE',  ( -1.000000000000000000, 0.000000000000000000, 0.000000000000000000 ) ) ;
#15464 = ADVANCED_FACE ( 'NONE', ( #2175 ), #2610, .F. ) ;
#15465 = LINE ( 'NONE', #5413, #13150 ) ;
#15466 = DIRECTION ( 'NONE',  ( 0.000000000000000000, 0.000000000000000000, -1.000000000000000000 ) ) ;
#15467 = CARTESIAN_POINT ( 'NONE',  ( 10.00000000000000000, 81.55207211302078463, -24.17537951050094236 ) ) ;
#15468 = CARTESIAN_POINT ( 'NONE',  ( 123.0000000000000000, 0.000000000000000000, -3.000000000000000000 ) ) ;
#15469 =( REPRESENTATION_RELATIONSHIP ('NONE','NONE', #2177, #21798 ) REPRESENTATION_RELATIONSHIP_WITH_TRANSFORMATION ( #11631 )SHAPE_REPRESENTATION_RELATIONSHIP( ) );
#15470 = CARTESIAN_POINT ( 'NONE',  ( 10.00000000000000000, 32.56745702629739014, 78.57830605990665163 ) ) ;
#15471 = ORIENTED_EDGE ( 'NONE', *, *, #21203, .F. ) ;
#15472 = DIRECTION ( 'NONE',  ( 1.000000000000000000, 0.000000000000000000, 0.000000000000000000 ) ) ;
#15473 = AXIS2_PLACEMENT_3D ( 'NONE', #12771, #11131, #5947 ) ;
#15474 = ORIENTED_EDGE ( 'NONE', *, *, #20788, .F. ) ;
#15475 = VECTOR ( 'NONE', #5298, 1000.000000000000000 ) ;
#15476 = CIRCLE ( 'NONE', #18319, 45.00000000000000000 ) ;
#15477 = ORIENTED_EDGE ( 'NONE', *, *, #9092, .T. ) ;
#15478 = CARTESIAN_POINT ( 'NONE',  ( 10.00000000000000000, 0.000000000000000000, 0.000000000000000000 ) ) ;
#15479 = ORIENTED_EDGE ( 'NONE', *, *, #15270, .F. ) ;
#15480 = VERTEX_POINT ( 'NONE', #14208 ) ;
#15481 = DIRECTION ( 'NONE',  ( 0.000000000000000000, 0.000000000000000000, 1.000000000000000000 ) ) ;
#15482 = EDGE_LOOP ( 'NONE', ( #7110, #20896, #11728, #1029 ) ) ;
#15483 = AXIS2_PLACEMENT_3D ( 'NONE', #17752, #11003, #6048 ) ;
#15484 = DIRECTION ( 'NONE',  ( 0.000000000000000000, 0.000000000000000000, 1.000000000000000000 ) ) ;
#15485 = CIRCLE ( 'NONE', #13353, 5.000000000000000000 ) ;
#15486 = CARTESIAN_POINT ( 'NONE',  ( -1.399999999999999911, 0.000000000000000000, 0.000000000000000000 ) ) ;
#15487 = DIRECTION ( 'NONE',  ( 1.000000000000000000, 0.000000000000000000, 0.000000000000000000 ) ) ;
#15488 = AXIS2_PLACEMENT_3D ( 'NONE', #21078, #4503, #21405 ) ;
#15489 = DIRECTION ( 'NONE',  ( 1.000000000000000000, -0.000000000000000000, -0.000000000000000000 ) ) ;
#15490 = VECTOR ( 'NONE', #16210, 1000.000000000000000 ) ;
#15491 = AXIS2_PLACEMENT_3D ( 'NONE', #10603, #17351, #14238 ) ;
#15492 = EDGE_CURVE ( 'NONE', #6690, #16592, #7055, .T. ) ;
#15493 = DIRECTION ( 'NONE',  ( 0.000000000000000000, -1.000000000000000000, 0.000000000000000000 ) ) ;
#15494 = CARTESIAN_POINT ( 'NONE',  ( 10.00000000000000000, 52.96496548042853192, 66.55750800669373746 ) ) ;
#15495 = CARTESIAN_POINT ( 'NONE',  ( 10.00000000000000000, 0.000000000000000000, 0.000000000000000000 ) ) ;
#15496 = ORIENTED_EDGE ( 'NONE', *, *, #11790, .F. ) ;
#15497 = CIRCLE ( 'NONE', #5983, 32.00000000000000000 ) ;
#15498 = DIRECTION ( 'NONE',  ( 1.000000000000000000, 0.000000000000000000, 0.000000000000000000 ) ) ;
#15499 = AXIS2_PLACEMENT_3D ( 'NONE', #13445, #11462, #11580 ) ;
#15500 = DIRECTION ( 'NONE',  ( 0.000000000000000000, 0.000000000000000000, 1.000000000000000000 ) ) ;
#15501 = VERTEX_POINT ( 'NONE', #7272 ) ;
#15502 = AXIS2_PLACEMENT_3D ( 'NONE', #7362, #12215, #11999 ) ;
#15503 = AXIS2_PLACEMENT_3D ( 'NONE', #12416, #13866, #19165 ) ;
#15504 = LINE ( 'NONE', #17379, #17139 ) ;
#15506 = AXIS2_PLACEMENT_3D ( 'NONE', #14678, #6307, #13024 ) ;
#15505 = PRODUCT_DEFINITION_SHAPE ( 'NONE', 'NONE',  #21858 ) ;
#15507 = ORIENTED_EDGE ( 'NONE', *, *, #8381, .F. ) ;
#15508 = DIRECTION ( 'NONE',  ( 0.000000000000000000, 0.000000000000000000, 1.000000000000000000 ) ) ;
#15509 = ORIENTED_EDGE ( 'NONE', *, *, #20268, .T. ) ;
#15510 = ADVANCED_FACE ( 'NONE', ( #20743 ), #11005, .F. ) ;
#15511 = VERTEX_POINT ( 'NONE', #14110 ) ;
#15512 = CARTESIAN_POINT ( 'NONE',  ( 0.000000000000000000, 0.000000000000000000, 0.000000000000000000 ) ) ;
#15513 = CYLINDRICAL_SURFACE ( 'NONE', #17726, 44.99999999999999289 ) ;
#15514 = DIRECTION ( 'NONE',  ( -1.000000000000000000, 0.000000000000000000, 0.000000000000000000 ) ) ;
#15515 = CARTESIAN_POINT ( 'NONE',  ( -10.00000000000000000, 0.000000000000000000, 0.000000000000000000 ) ) ;
#15516 = CARTESIAN_POINT ( 'NONE',  ( 5.000000000000000000, 56.05743251323859511, 67.83483072893820065 ) ) ;
#15517 = DIRECTION ( 'NONE',  ( 1.000000000000000000, 0.000000000000000000, 0.000000000000000000 ) ) ;
#15518 = EDGE_CURVE ( 'NONE', #16668, #11869, #11268, .T. ) ;
#15519 = DIRECTION ( 'NONE',  ( -1.000000000000000000, 0.000000000000000000, 0.000000000000000000 ) ) ;
#15520 = DIRECTION ( 'NONE',  ( 0.000000000000000000, 0.000000000000000000, 1.000000000000000000 ) ) ;
#15521 = AXIS2_PLACEMENT_3D ( 'NONE', #14629, #8009, #16065 ) ;
#15522 = VERTEX_POINT ( 'NONE', #7482 ) ;
#15523 = VECTOR ( 'NONE', #12880, 1000.000000000000000 ) ;
#15524 = DIRECTION ( 'NONE',  ( 0.000000000000000000, 0.000000000000000000, 1.000000000000000000 ) ) ;
#15525 = ADVANCED_FACE ( 'NONE', ( #20956 ), #9017, .T. ) ;
#15526 = ORIENTED_EDGE ( 'NONE', *, *, #18562, .T. ) ;
#15527 = DIRECTION ( 'NONE',  ( 1.000000000000000000, 0.000000000000000000, 0.000000000000000000 ) ) ;
#15528 = ORIENTED_EDGE ( 'NONE', *, *, #17215, .F. ) ;
#15529 = DIRECTION ( 'NONE',  ( -1.000000000000000000, -0.000000000000000000, 0.000000000000000000 ) ) ;
#15530 = DIRECTION ( 'NONE',  ( 0.000000000000000000, 0.2079116908177532363, 0.9781476007338069101 ) ) ;
#15531 = VERTEX_POINT ( 'NONE', #13998 ) ;
#15533 = EDGE_CURVE ( 'NONE', #3248, #18016, #15141, .T. ) ;
#15532 = VERTEX_POINT ( 'NONE', #5613 ) ;
#15534 = VERTEX_POINT ( 'NONE', #3944 ) ;
#15535 = EDGE_CURVE ( 'NONE', #11159, #5897, #17652, .T. ) ;
#15536 = ORIENTED_EDGE ( 'NONE', *, *, #1491, .F. ) ;
#15537 = EDGE_CURVE ( 'NONE', #14927, #16153, #14088, .T. ) ;
#15538 = AXIS2_PLACEMENT_3D ( 'NONE', #4225, #9182, #10957 ) ;
#15539 = DIRECTION ( 'NONE',  ( 1.000000000000000000, 0.000000000000000000, 0.000000000000000000 ) ) ;
#15540 = ORIENTED_EDGE ( 'NONE', *, *, #2990, .T. ) ;
#15541 = CARTESIAN_POINT ( 'NONE',  ( 10.00000000000000000, 83.48638250753229784, 27.82128566055142826 ) ) ;
#15542 = EDGE_CURVE ( 'NONE', #4811, #15448, #18981, .T. ) ;
#15543 = FACE_OUTER_BOUND ( 'NONE', #7602, .T. ) ;
#15544 = CARTESIAN_POINT ( 'NONE',  ( 0.000000000000000000, -61.71252885873347793, -58.53847642588656441 ) ) ;
#15545 = DIRECTION ( 'NONE',  ( 1.000000000000000000, 0.000000000000000000, 0.000000000000000000 ) ) ;
#15546 = CARTESIAN_POINT ( 'NONE',  ( 10.00000000000000000, 84.12297548659704205, 12.59025161327141618 ) ) ;
#15547 = CARTESIAN_POINT ( 'NONE',  ( 0.000000000000000000, 43.18649929580291058, -73.28107340219372645 ) ) ;
#15548 = FACE_OUTER_BOUND ( 'NONE', #18843, .T. ) ;
#15549 = VERTEX_POINT ( 'NONE', #12663 ) ;
#15550 = CARTESIAN_POINT ( 'NONE',  ( 10.00000000000000000, -65.64563793391867819, 54.09103124042793098 ) ) ;
#15551 = EDGE_CURVE ( 'NONE', #9664, #21294, #9144, .T. ) ;
#15552 = CARTESIAN_POINT ( 'NONE',  ( -1.500000000000001332, 0.000000000000000000, 0.000000000000000000 ) ) ;
#15553 = AXIS2_PLACEMENT_3D ( 'NONE', #3109, #10062, #9843 ) ;
#15554 = EDGE_CURVE ( 'NONE', #15334, #8596, #5715, .T. ) ;
#15555 = DIRECTION ( 'NONE',  ( 0.000000000000000000, -0.5877852522924632561, -0.8090169943749546677 ) ) ;
#15556 = ORIENTED_EDGE ( 'NONE', *, *, #12994, .T. ) ;
#15557 = DIRECTION ( 'NONE',  ( 0.000000000000000000, 0.000000000000000000, -1.000000000000000000 ) ) ;
#15558 = VERTEX_POINT ( 'NONE', #7383 ) ;
#15559 = DIRECTION ( 'NONE',  ( -1.000000000000000000, 0.000000000000000000, 0.000000000000000000 ) ) ;
#15560 = VERTEX_POINT ( 'NONE', #17541 ) ;
#15561 = ORIENTED_EDGE ( 'NONE', *, *, #14960, .T. ) ;
#15562 = ORIENTED_EDGE ( 'NONE', *, *, #1528, .T. ) ;
#15563 = DIRECTION ( 'NONE',  ( 1.000000000000000000, 0.000000000000000000, 0.000000000000000000 ) ) ;
#15564 = EDGE_CURVE ( 'NONE', #9611, #3591, #13885, .T. ) ;
#15565 = CARTESIAN_POINT ( 'NONE',  ( 10.00000000000000000, -90.32141448704695108, 19.96189084378191936 ) ) ;
#15566 = CARTESIAN_POINT ( 'NONE',  ( 5.000000000000000000, -61.60362715318993310, -62.84101464466307618 ) ) ;
#15567 = AXIS2_PLACEMENT_3D ( 'NONE', #21837, #20187, #17085 ) ;
#15568 = FACE_OUTER_BOUND ( 'NONE', #8723, .T. ) ;
#15569 = PRODUCT_DEFINITION_CONTEXT ( 'detailed design', #17729, 'design' ) ;
#15570 = CARTESIAN_POINT ( 'NONE',  ( 10.00000000000000000, 68.36541360927188293, 50.60987712331726840 ) ) ;
#15571 = DIRECTION ( 'NONE',  ( 1.000000000000000000, -0.000000000000000000, -0.000000000000000000 ) ) ;
#15572 = DIRECTION ( 'NONE',  ( 1.000000000000000000, 0.000000000000000000, 0.000000000000000000 ) ) ;
#15573 = DIRECTION ( 'NONE',  ( 0.000000000000000000, 0.000000000000000000, -1.000000000000000000 ) ) ;
#15574 = CARTESIAN_POINT ( 'NONE',  ( 5.000000000000000000, 24.17932380791719282, 20.96092317127012805 ) ) ;
#15575 = ADVANCED_FACE ( 'NONE', ( #2502 ), #9228, .T. ) ;
#15576 = EDGE_LOOP ( 'NONE', ( #11779, #1709 ) ) ;
#15577 = EDGE_CURVE ( 'NONE', #6845, #8545, #19757, .T. ) ;
#15578 = FACE_OUTER_BOUND ( 'NONE', #10477, .T. ) ;
#15579 = VERTEX_POINT ( 'NONE', #19511 ) ;
#15580 = AXIS2_PLACEMENT_3D ( 'NONE', #4559, #12944, #2559 ) ;
#15581 = ORIENTED_EDGE ( 'NONE', *, *, #5698, .F. ) ;
#15582 = EDGE_CURVE ( 'NONE', #20085, #16931, #4380, .T. ) ;
#15583 = ADVANCED_FACE ( 'NONE', ( #3054 ), #13202, .F. ) ;
#15584 = ORIENTED_EDGE ( 'NONE', *, *, #12735, .F. ) ;
#15585 = CARTESIAN_POINT ( 'NONE',  ( 10.00000000000000000, 0.000000000000000000, 0.000000000000000000 ) ) ;
#15586 = VERTEX_POINT ( 'NONE', #11120 ) ;
#15587 = ORIENTED_EDGE ( 'NONE', *, *, #14061, .F. ) ;
#15588 = DIRECTION ( 'NONE',  ( -1.000000000000000000, -0.000000000000000000, -0.000000000000000000 ) ) ;
#15589 = EDGE_LOOP ( 'NONE', ( #12860, #7619, #17254, #4251 ) ) ;
#15590 = DIRECTION ( 'NONE',  ( 1.000000000000000000, 0.000000000000000000, 0.000000000000000000 ) ) ;
#15591 = DIRECTION ( 'NONE',  ( 0.000000000000000000, -0.3420201433256569445, -0.9396926207859125357 ) ) ;
#15592 = DIRECTION ( 'NONE',  ( 0.000000000000000000, 0.000000000000000000, -1.000000000000000000 ) ) ;
#15593 = DIRECTION ( 'NONE',  ( 0.000000000000000000, 0.000000000000000000, 1.000000000000000000 ) ) ;
#15594 = LINE ( 'NONE', #8535, #14323 ) ;
#15595 = EDGE_LOOP ( 'NONE', ( #15807, #3143, #13390, #19306 ) ) ;
#15596 = DIRECTION ( 'NONE',  ( -1.000000000000000000, 0.000000000000000000, 0.000000000000000000 ) ) ;
#15597 = CARTESIAN_POINT ( 'NONE',  ( -1.399999999999998579, 6.184466335694134054E-16, 5.000000000000000888 ) ) ;
#15598 = DIRECTION ( 'NONE',  ( 1.000000000000000000, 0.000000000000000000, 0.000000000000000000 ) ) ;
#15599 = ORIENTED_EDGE ( 'NONE', *, *, #13407, .F. ) ;
#15600 = CIRCLE ( 'NONE', #19483, 44.99999999999999289 ) ;
#15601 = CARTESIAN_POINT ( 'NONE',  ( 5.000000000000000000, 81.34229909304679040, 33.57723005635394742 ) ) ;
#15602 = DIRECTION ( 'NONE',  ( 0.000000000000000000, -1.000000000000000000, 0.000000000000000000 ) ) ;
#15603 = ORIENTED_EDGE ( 'NONE', *, *, #12033, .T. ) ;
#15604 = DIRECTION ( 'NONE',  ( 0.000000000000000000, -0.06975647374413236623, 0.9975640502598237536 ) ) ;
#15605 = ORIENTED_EDGE ( 'NONE', *, *, #7337, .T. ) ;
#15606 = DIRECTION ( 'NONE',  ( 1.000000000000000000, 0.000000000000000000, 0.000000000000000000 ) ) ;
#15607 = CIRCLE ( 'NONE', #10653, 88.00000000000000000 ) ;
#15608 = VERTEX_POINT ( 'NONE', #8031 ) ;
#15609 = ORIENTED_EDGE ( 'NONE', *, *, #5535, .F. ) ;
#15610 = CARTESIAN_POINT ( 'NONE',  ( 10.00000000000000000, 0.000000000000000000, 0.000000000000000000 ) ) ;
#15611 = CARTESIAN_POINT ( 'NONE',  ( 10.00000000000000000, -51.10509369859486384, 77.10190917907182495 ) ) ;
#15612 = AXIS2_PLACEMENT_3D ( 'NONE', #226, #11610, #13255 ) ;
#15613 = CARTESIAN_POINT ( 'NONE',  ( 5.000000000000002665, -87.96697768756401103, -2.410567674971490604 ) ) ;
#15614 = LINE ( 'NONE', #3586, #11929 ) ;
#15615 = FACE_OUTER_BOUND ( 'NONE', #18931, .T. ) ;
#15616 = DIRECTION ( 'NONE',  ( 0.000000000000000000, -0.5299192642332118952, 0.8480480961564216269 ) ) ;
#15617 = CIRCLE ( 'NONE', #17746, 2.799999999999996714 ) ;
#15618 = DIRECTION ( 'NONE',  ( 1.000000000000000000, 0.000000000000000000, 0.000000000000000000 ) ) ;
#15619 = DIRECTION ( 'NONE',  ( 1.000000000000000000, 0.000000000000000000, 0.000000000000000000 ) ) ;
#15620 = ORIENTED_EDGE ( 'NONE', *, *, #7088, .T. ) ;
#15621 = LINE ( 'NONE', #19159, #16788 ) ;
#15622 = CIRCLE ( 'NONE', #7855, 2.799999999999996714 ) ;
#15623 = ADVANCED_FACE ( 'NONE', ( #18080, #7697 ), #1406, .T. ) ;
#15624 = ORIENTED_EDGE ( 'NONE', *, *, #72, .T. ) ;
#15625 = CYLINDRICAL_SURFACE ( 'NONE', #20389, 27.49900000000000233 ) ;
#15626 = VERTEX_POINT ( 'NONE', #9444 ) ;
#15627 = CIRCLE ( 'NONE', #9259, 45.00000000000000000 ) ;
#15628 = AXIS2_PLACEMENT_3D ( 'NONE', #2855, #4183, #10918 ) ;
#15629 = CYLINDRICAL_SURFACE ( 'NONE', #14450, 5.612499999999999822 ) ;
#15630 = CARTESIAN_POINT ( 'NONE',  ( 0.000000000000000000, 0.000000000000000000, 0.000000000000000000 ) ) ;
#15631 = EDGE_LOOP ( 'NONE', ( #19192, #16671, #5580, #18536 ) ) ;
#15632 = EDGE_CURVE ( 'NONE', #19849, #10985, #11562, .T. ) ;
#15633 = AXIS2_PLACEMENT_3D ( 'NONE', #1916, #15606, #13844 ) ;
#15634 =( LENGTH_UNIT ( ) NAMED_UNIT ( * ) SI_UNIT ( .MILLI., .METRE. ) );
#15635 = ORIENTED_EDGE ( 'NONE', *, *, #17759, .T. ) ;
#15636 = VERTEX_POINT ( 'NONE', #7916 ) ;
#15637 = ORIENTED_EDGE ( 'NONE', *, *, #16228, .T. ) ;
#15638 = CARTESIAN_POINT ( 'NONE',  ( 0.000000000000000000, 0.000000000000000000, 0.000000000000000000 ) ) ;
#15639 = ORIENTED_EDGE ( 'NONE', *, *, #18884, .F. ) ;
#15640 = CIRCLE ( 'NONE', #8584, 11.99999999999999822 ) ;
#15641 = LINE ( 'NONE', #512, #9311 ) ;
#15642 = CARTESIAN_POINT ( 'NONE',  ( 10.00000000000000000, 0.000000000000000000, 0.000000000000000000 ) ) ;
#15643 = CARTESIAN_POINT ( 'NONE',  ( 10.00000000000000000, -4.294029059349679045, -27.86182539015970505 ) ) ;
#15644 = DIRECTION ( 'NONE',  ( 1.000000000000000000, 0.000000000000000000, 0.000000000000000000 ) ) ;
#15645 = DIRECTION ( 'NONE',  ( -3.552713678800500929E-15, -1.000000000000000000, 0.000000000000000000 ) ) ;
#15646 = DIRECTION ( 'NONE',  ( -1.000000000000000000, -0.000000000000000000, -0.000000000000000000 ) ) ;
#15647 = ORIENTED_EDGE ( 'NONE', *, *, #6275, .F. ) ;
#15648 = AXIS2_PLACEMENT_3D ( 'NONE', #9188, #2560, #21243 ) ;
#15649 = DIRECTION ( 'NONE',  ( -1.000000000000000000, -0.000000000000000000, -0.000000000000000000 ) ) ;
#15650 = DIRECTION ( 'NONE',  ( -1.000000000000000000, -0.000000000000000000, 0.000000000000000000 ) ) ;
#15651 = EDGE_CURVE ( 'NONE', #6083, #11017, #359, .T. ) ;
#15652 = EDGE_CURVE ( 'NONE', #7603, #15964, #19043, .T. ) ;
#15653 = EDGE_CURVE ( 'NONE', #21244, #21645, #8468, .T. ) ;
#15654 = CARTESIAN_POINT ( 'NONE',  ( 0.000000000000000000, -15.51843147776405729, 83.63233659819645993 ) ) ;
#15655 = ORIENTED_EDGE ( 'NONE', *, *, #13130, .F. ) ;
#15656 = EDGE_CURVE ( 'NONE', #993, #19336, #1419, .T. ) ;
#15657 = AXIS2_PLACEMENT_3D ( 'NONE', #3724, #18656, #8898 ) ;
#15658 = DIRECTION ( 'NONE',  ( -1.000000000000000000, 0.000000000000000000, 0.000000000000000000 ) ) ;
#15659 = ORIENTED_EDGE ( 'NONE', *, *, #9044, .T. ) ;
#15660 = CARTESIAN_POINT ( 'NONE',  ( 10.00000000000000000, 84.80486432185243473, -36.94008646920313055 ) ) ;
#15661 = ORIENTED_EDGE ( 'NONE', *, *, #14465, .T. ) ;
#15662 = CIRCLE ( 'NONE', #2954, 88.00000000000000000 ) ;
#15663 = VERTEX_POINT ( 'NONE', #21513 ) ;
#15664 = VERTEX_POINT ( 'NONE', #9552 ) ;
#15665 = CARTESIAN_POINT ( 'NONE',  ( 150.0000507999999968, 0.000000000000000000, 3.000000000000000444 ) ) ;
#15666 = CIRCLE ( 'NONE', #2958, 88.00000000000000000 ) ;
#15667 = VERTEX_POINT ( 'NONE', #6051 ) ;
#15668 = EDGE_CURVE ( 'NONE', #11004, #17333, #5642, .T. ) ;
#15669 = CARTESIAN_POINT ( 'NONE',  ( 10.00000000000000000, 0.000000000000000000, 0.000000000000000000 ) ) ;
#15670 = CARTESIAN_POINT ( 'NONE',  ( 5.000000000000000888, -31.75612719289738095, -3.943144139962873940 ) ) ;
#15671 = CARTESIAN_POINT ( 'NONE',  ( 0.000000000000000000, 0.000000000000000000, 3.000000000000000000 ) ) ;
#15672 = PRESENTATION_STYLE_ASSIGNMENT (( #15342 ) ) ;
#15673 = EDGE_CURVE ( 'NONE', #16358, #15586, #20472, .T. ) ;
#15674 = CIRCLE ( 'NONE', #4386, 0.02569999999999482421 ) ;
#15675 = CARTESIAN_POINT ( 'NONE',  ( 0.000000000000000000, 89.12061559554365431, -24.77803214283454736 ) ) ;
#15676 = DIRECTION ( 'NONE',  ( 0.000000000000000000, 0.000000000000000000, 1.000000000000000000 ) ) ;
#15677 = CARTESIAN_POINT ( 'NONE',  ( -1.200000000000006617, 0.000000000000000000, 0.000000000000000000 ) ) ;
#15678 = FACE_OUTER_BOUND ( 'NONE', #15751, .T. ) ;
#15679 = CARTESIAN_POINT ( 'NONE',  ( 10.00000000000000000, 0.000000000000000000, 0.000000000000000000 ) ) ;
#15680 = AXIS2_PLACEMENT_3D ( 'NONE', #14533, #19944, #21275 ) ;
#15681 = ADVANCED_FACE ( 'NONE', ( #4703 ), #954, .T. ) ;
#15682 = ORIENTED_EDGE ( 'NONE', *, *, #8255, .F. ) ;
#15683 = AXIS2_PLACEMENT_3D ( 'NONE', #3904, #20815, #20592 ) ;
#15684 = DIRECTION ( 'NONE',  ( -1.000000000000000000, 0.000000000000000000, 0.000000000000000000 ) ) ;
#15685 = ORIENTED_EDGE ( 'NONE', *, *, #17493, .T. ) ;
#15686 = EDGE_CURVE ( 'NONE', #1324, #18185, #14540, .T. ) ;
#15687 = EDGE_LOOP ( 'NONE', ( #4097, #18966, #20242, #299 ) ) ;
#15688 = VERTEX_POINT ( 'NONE', #4603 ) ;
#15689 = DIRECTION ( 'NONE',  ( 1.000000000000000000, 0.000000000000000000, 0.000000000000000000 ) ) ;
#15690 = AXIS2_PLACEMENT_3D ( 'NONE', #11194, #8512, #15235 ) ;
#15691 = ORIENTED_EDGE ( 'NONE', *, *, #6776, .T. ) ;
#15692 = AXIS2_PLACEMENT_3D ( 'NONE', #9691, #6417, #9922 ) ;
#15693 = ORIENTED_EDGE ( 'NONE', *, *, #7594, .F. ) ;
#15694 = CIRCLE ( 'NONE', #15745, 44.99999999999999289 ) ;
#15695 = EDGE_CURVE ( 'NONE', #6705, #20437, #11444, .T. ) ;
#15696 = VECTOR ( 'NONE', #18188, 1000.000000000000000 ) ;
#15697 = DIRECTION ( 'NONE',  ( -1.000000000000000000, -0.000000000000000000, -0.000000000000000000 ) ) ;
#15698 = ORIENTED_EDGE ( 'NONE', *, *, #7826, .F. ) ;
#15699 = EDGE_CURVE ( 'NONE', #2112, #19416, #3528, .T. ) ;
#15700 = CARTESIAN_POINT ( 'NONE',  ( 0.000000000000000000, -33.95793648385753727, -86.04239391578025220 ) ) ;
#15701 = AXIS2_PLACEMENT_3D ( 'NONE', #16600, #18778, #3859 ) ;
#15702 = LINE ( 'NONE', #20679, #448 ) ;
#15703 = CYLINDRICAL_SURFACE ( 'NONE', #1601, 27.49900000000000233 ) ;
#15704 = CYLINDRICAL_SURFACE ( 'NONE', #21274, 88.00000000000000000 ) ;
#15705 = DIRECTION ( 'NONE',  ( -1.000000000000000000, 0.000000000000000000, -0.000000000000000000 ) ) ;
#15706 = ADVANCED_FACE ( 'NONE', ( #284 ), #18521, .F. ) ;
#15707 = ADVANCED_FACE ( 'NONE', ( #3592 ), #1610, .F. ) ;
#15708 = DIRECTION ( 'NONE',  ( -1.000000000000000000, 0.000000000000000000, 0.000000000000000000 ) ) ;
#15709 = CARTESIAN_POINT ( 'NONE',  ( 10.00000000000000000, 26.27606311335951617, 10.21217444509420424 ) ) ;
#15710 = LINE ( 'NONE', #21011, #2080 ) ;
#15711 = AXIS2_PLACEMENT_3D ( 'NONE', #13171, #2907, #21796 ) ;
#15712 = CIRCLE ( 'NONE', #11123, 6.728125000000023448 ) ;
#15713 = ORIENTED_EDGE ( 'NONE', *, *, #2138, .T. ) ;
#15714 = AXIS2_PLACEMENT_3D ( 'NONE', #15933, #9286, #14160 ) ;
#15715 = AXIS2_PLACEMENT_3D ( 'NONE', #18976, #1958, #3936 ) ;
#15716 = VECTOR ( 'NONE', #5223, 1000.000000000000000 ) ;
#15717 = EDGE_CURVE ( 'NONE', #7130, #15626, #10227, .T. ) ;
#15718 = DIRECTION ( 'NONE',  ( -1.000000000000000000, 0.000000000000000000, -0.000000000000000000 ) ) ;
#15719 = DIRECTION ( 'NONE',  ( 0.000000000000000000, 0.000000000000000000, -1.000000000000000000 ) ) ;
#15720 = ORIENTED_EDGE ( 'NONE', *, *, #14112, .T. ) ;
#15721 = AXIS2_PLACEMENT_3D ( 'NONE', #14959, #380, #7120 ) ;
#15722 = CARTESIAN_POINT ( 'NONE',  ( 10.00000000000000000, 8.134922360106093819, 84.67002113262482510 ) ) ;
#15723 = ORIENTED_EDGE ( 'NONE', *, *, #14179, .F. ) ;
#15724 =( NAMED_UNIT ( * ) SI_UNIT ( $, .STERADIAN. ) SOLID_ANGLE_UNIT ( ) );
#15725 = DIRECTION ( 'NONE',  ( 1.000000000000000000, 0.000000000000000000, 0.000000000000000000 ) ) ;
#15726 = ORIENTED_EDGE ( 'NONE', *, *, #4003, .T. ) ;
#15727 = AXIS2_PLACEMENT_3D ( 'NONE', #21333, #6216, #16475 ) ;
#15728 = ORIENTED_EDGE ( 'NONE', *, *, #7705, .T. ) ;
#15729 = DIRECTION ( 'NONE',  ( 0.000000000000000000, 0.000000000000000000, 1.000000000000000000 ) ) ;
#15730 = CIRCLE ( 'NONE', #166, 44.99999999999999289 ) ;
#15731 = AXIS2_PLACEMENT_3D ( 'NONE', #1926, #5358, #18625 ) ;
#15732 = DIRECTION ( 'NONE',  ( -1.000000000000000000, -0.000000000000000000, -0.000000000000000000 ) ) ;
#15733 = DIRECTION ( 'NONE',  ( 0.000000000000000000, -1.000000000000000000, 0.000000000000000000 ) ) ;
#15734 = CARTESIAN_POINT ( 'NONE',  ( 10.00000000000000000, -64.66851233300690183, -55.25552418573029456 ) ) ;
#15735 = DIRECTION ( 'NONE',  ( 1.000000000000000000, -0.000000000000000000, 0.000000000000000000 ) ) ;
#15736 = ADVANCED_FACE ( 'NONE', ( #16970 ), #21715, .T. ) ;
#15737 = FACE_OUTER_BOUND ( 'NONE', #19470, .T. ) ;
#15738 = DIRECTION ( 'NONE',  ( -1.000000000000000000, -0.000000000000000000, -0.000000000000000000 ) ) ;
#15739 = ORIENTED_EDGE ( 'NONE', *, *, #5288, .F. ) ;
#15740 = DIRECTION ( 'NONE',  ( 1.000000000000000000, -0.000000000000000000, 0.000000000000000000 ) ) ;
#15741 = EDGE_LOOP ( 'NONE', ( #8221, #18452, #16456, #4415 ) ) ;
#15742 = CIRCLE ( 'NONE', #19626, 44.99999999999999289 ) ;
#15743 = AXIS2_PLACEMENT_3D ( 'NONE', #3339, #2126, #17268 ) ;
#15744 = CARTESIAN_POINT ( 'NONE',  ( 0.000000000000000000, 11.59241532900628258, 87.23311244498744088 ) ) ;
#15745 = AXIS2_PLACEMENT_3D ( 'NONE', #2740, #9463, #4619 ) ;
#15746 = VERTEX_POINT ( 'NONE', #3375 ) ;
#15747 = CARTESIAN_POINT ( 'NONE',  ( 0.000000000000000000, 52.25832601289194201, -70.80301803122729609 ) ) ;
#15748 = FACE_OUTER_BOUND ( 'NONE', #12219, .T. ) ;
#15749 = ORIENTED_EDGE ( 'NONE', *, *, #3112, .F. ) ;
#15750 =( LENGTH_UNIT ( ) NAMED_UNIT ( * ) SI_UNIT ( .MILLI., .METRE. ) );
#15751 = EDGE_LOOP ( 'NONE', ( #5779, #16958, #812, #13134 ) ) ;
#15752 = EDGE_LOOP ( 'NONE', ( #6375, #6259, #18205, #20926 ) ) ;
#15753 = VERTEX_POINT ( 'NONE', #13430 ) ;
#15754 = DIRECTION ( 'NONE',  ( 1.000000000000000000, 0.000000000000000000, 0.000000000000000000 ) ) ;
#15755 = CARTESIAN_POINT ( 'NONE',  ( -1.139999999999998570, 0.000000000000000000, 0.000000000000000000 ) ) ;
#15756 = VERTEX_POINT ( 'NONE', #6925 ) ;
#15757 = DIRECTION ( 'NONE',  ( 0.000000000000000000, 0.000000000000000000, 1.000000000000000000 ) ) ;
#15758 = PLANE ( 'NONE',  #13325 ) ;
#15759 = EDGE_CURVE ( 'NONE', #12763, #5686, #15410, .T. ) ;
#15760 = DIRECTION ( 'NONE',  ( 0.000000000000000000, 0.000000000000000000, -1.000000000000000000 ) ) ;
#15761 = DIRECTION ( 'NONE',  ( 1.000000000000000000, 0.000000000000000000, 0.000000000000000000 ) ) ;
#15762 = STYLED_ITEM ( 'NONE', ( #9829 ), #13597 ) ;
#15763 = CARTESIAN_POINT ( 'NONE',  ( 10.00000000000000000, -25.56104204395249369, -81.12843256239690959 ) ) ;
#15764 = VERTEX_POINT ( 'NONE', #11674 ) ;
#15765 = CARTESIAN_POINT ( 'NONE',  ( 5.000000000000000888, 30.24235385705252099, -10.45944707835077558 ) ) ;
#15766 = DIRECTION ( 'NONE',  ( -1.000000000000000000, 0.000000000000000000, 0.000000000000000000 ) ) ;
#15767 = CARTESIAN_POINT ( 'NONE',  ( 10.00000000000000000, -39.87723064937059547, -83.46401306393613595 ) ) ;
#15768 = ORIENTED_EDGE ( 'NONE', *, *, #18128, .T. ) ;
#15769 = AXIS2_PLACEMENT_3D ( 'NONE', #8839, #1991, #15573 ) ;
#15770 = DIRECTION ( 'NONE',  ( 0.000000000000000000, 0.000000000000000000, 1.000000000000000000 ) ) ;
#15771 = CIRCLE ( 'NONE', #12940, 88.00000000000000000 ) ;
#15772 = ORIENTED_EDGE ( 'NONE', *, *, #5820, .T. ) ;
#15773 = DIRECTION ( 'NONE',  ( 0.000000000000000000, 0.9510565162951544194, -0.3090169943749449533 ) ) ;
#15774 = AXIS2_PLACEMENT_3D ( 'NONE', #14349, #9042, #5521 ) ;
#15775 = ORIENTED_EDGE ( 'NONE', *, *, #4622, .T. ) ;
#15776 = ORIENTED_EDGE ( 'NONE', *, *, #7471, .F. ) ;
#15777 = ORIENTED_EDGE ( 'NONE', *, *, #19730, .T. ) ;
#15778 = CYLINDRICAL_SURFACE ( 'NONE', #17871, 88.00000000000000000 ) ;
#15779 = ORIENTED_EDGE ( 'NONE', *, *, #10146, .F. ) ;
#15780 = DIRECTION ( 'NONE',  ( 0.000000000000000000, 1.224646799147353947E-16, 1.000000000000000000 ) ) ;
#15781 = DIRECTION ( 'NONE',  ( 0.000000000000000000, 0.000000000000000000, 1.000000000000000000 ) ) ;
#15782 = FACE_OUTER_BOUND ( 'NONE', #17466, .T. ) ;
#15783 = EDGE_CURVE ( 'NONE', #18185, #16931, #6011, .T. ) ;
#15784 = DIRECTION ( 'NONE',  ( -1.000000000000000000, 0.000000000000000000, -0.000000000000000000 ) ) ;
#15785 = AXIS2_PLACEMENT_3D ( 'NONE', #14677, #12909, #19767 ) ;
#15786 = CARTESIAN_POINT ( 'NONE',  ( -10.00000000000000000, 0.000000000000000000, 0.000000000000000000 ) ) ;
#15787 = AXIS2_PLACEMENT_3D ( 'NONE', #1940, #13764, #3702 ) ;
#15788 = LINE ( 'NONE', #20869, #2718 ) ;
#15789 = DIRECTION ( 'NONE',  ( -1.000000000000000000, -0.000000000000000000, 0.000000000000000000 ) ) ;
#15790 = CIRCLE ( 'NONE', #10489, 44.99999999999998579 ) ;
#15791 = CYLINDRICAL_SURFACE ( 'NONE', #9075, 44.99999999999999289 ) ;
#15792 = FACE_OUTER_BOUND ( 'NONE', #5944, .T. ) ;
#15793 = EDGE_LOOP ( 'NONE', ( #20357, #20141, #13520, #6036 ) ) ;
#15794 = CYLINDRICAL_SURFACE ( 'NONE', #20347, 27.49900000000000233 ) ;
#15795 = EDGE_CURVE ( 'NONE', #9608, #1843, #4940, .T. ) ;
#15796 = ORIENTED_EDGE ( 'NONE', *, *, #4777, .F. ) ;
#15797 = ORIENTED_EDGE ( 'NONE', *, *, #6411, .T. ) ;
#15798 = ORIENTED_EDGE ( 'NONE', *, *, #6760, .F. ) ;
#15799 = AXIS2_PLACEMENT_3D ( 'NONE', #13389, #20139, #4993 ) ;
#15800 = LINE ( 'NONE', #18092, #14841 ) ;
#15801 = CIRCLE ( 'NONE', #2394, 11.99999999999999645 ) ;
#15802 = ORIENTED_EDGE ( 'NONE', *, *, #7980, .F. ) ;
#15803 = VECTOR ( 'NONE', #6365, 1000.000000000000000 ) ;
#15804 = AXIS2_PLACEMENT_3D ( 'NONE', #14427, #21391, #6045 ) ;
#15805 = ORIENTED_EDGE ( 'NONE', *, *, #1748, .T. ) ;
#15806 = AXIS2_PLACEMENT_3D ( 'NONE', #16947, #5339, #3780 ) ;
#15807 = ORIENTED_EDGE ( 'NONE', *, *, #12828, .F. ) ;
#15808 = DIRECTION ( 'NONE',  ( 1.000000000000000000, -0.000000000000000000, 0.000000000000000000 ) ) ;
#15809 = ADVANCED_FACE ( 'NONE', ( #18419 ), #13648, .F. ) ;
#15810 = ORIENTED_EDGE ( 'NONE', *, *, #5191, .F. ) ;
#15811 = EDGE_CURVE ( 'NONE', #10685, #18258, #12339, .T. ) ;
#15812 = EDGE_CURVE ( 'NONE', #2555, #11833, #17648, .T. ) ;
#15813 = CARTESIAN_POINT ( 'NONE',  ( 0.000000000000000000, -76.53853822673953289, -43.42639941457193231 ) ) ;
#15814 = CARTESIAN_POINT ( 'NONE',  ( 10.00000000000000000, 0.000000000000000000, 0.000000000000000000 ) ) ;
#15815 = CIRCLE ( 'NONE', #14044, 1.100000000000003642 ) ;
#15816 = EDGE_CURVE ( 'NONE', #10938, #1, #20810, .T. ) ;
#15817 = CARTESIAN_POINT ( 'NONE',  ( 10.00000000000000000, 0.000000000000000000, 0.000000000000000000 ) ) ;
#15818 = CARTESIAN_POINT ( 'NONE',  ( 0.000000000000000000, -85.05652083079337444, 0.7600687895857258791 ) ) ;
#15819 = DIRECTION ( 'NONE',  ( 1.000000000000000000, 0.000000000000000000, 0.000000000000000000 ) ) ;
#15820 = CARTESIAN_POINT ( 'NONE',  ( 0.000000000000000000, 0.000000000000000000, 0.000000000000000000 ) ) ;
#15821 = LINE ( 'NONE', #5660, #12613 ) ;
#15822 = DIRECTION ( 'NONE',  ( 0.000000000000000000, 0.000000000000000000, 1.000000000000000000 ) ) ;
#15823 = AXIS2_PLACEMENT_3D ( 'NONE', #5873, #16130, #12592 ) ;
#15824 = ADVANCED_FACE ( 'NONE', ( #20398 ), #10110, .F. ) ;
#15825 = AXIS2_PLACEMENT_3D ( 'NONE', #8499, #425, #20438 ) ;
#15826 = CIRCLE ( 'NONE', #21474, 44.99999999999999289 ) ;
#15827 = ORIENTED_EDGE ( 'NONE', *, *, #4906, .F. ) ;
#15828 = AXIS2_PLACEMENT_3D ( 'NONE', #3207, #4875, #18365 ) ;
#15829 = DIRECTION ( 'NONE',  ( -1.000000000000000000, -0.000000000000000000, 0.000000000000000000 ) ) ;
#15830 = EDGE_CURVE ( 'NONE', #13720, #874, #560, .T. ) ;
#15831 = DIRECTION ( 'NONE',  ( 1.000000000000000000, 0.000000000000000000, 0.000000000000000000 ) ) ;
#15832 = ADVANCED_FACE ( 'NONE', ( #1498 ), #8240, .T. ) ;
#15833 = CARTESIAN_POINT ( 'NONE',  ( 10.00000000000000000, -81.97107881582179800, -22.71412948308650925 ) ) ;
#15834 = ORIENTED_EDGE ( 'NONE', *, *, #18418, .T. ) ;
#15835 = DIRECTION ( 'NONE',  ( -1.000000000000000000, 0.000000000000000000, -0.000000000000000000 ) ) ;
#15836 = ORIENTED_EDGE ( 'NONE', *, *, #21727, .T. ) ;
#15837 = EDGE_CURVE ( 'NONE', #12265, #17743, #17155, .T. ) ;
#15838 = AXIS2_PLACEMENT_3D ( 'NONE', #20644, #17118, #7168 ) ;
#15839 = FACE_OUTER_BOUND ( 'NONE', #14293, .T. ) ;
#15840 = ORIENTED_EDGE ( 'NONE', *, *, #14488, .T. ) ;
#15841 = CIRCLE ( 'NONE', #19029, 88.00000000000000000 ) ;
#15842 = ORIENTED_EDGE ( 'NONE', *, *, #2138, .F. ) ;
#15843 = CARTESIAN_POINT ( 'NONE',  ( 0.000000000000000000, 0.000000000000000000, 0.000000000000000000 ) ) ;
#15844 = AXIS2_PLACEMENT_3D ( 'NONE', #8715, #15010, #17332 ) ;
#15845 = CIRCLE ( 'NONE', #1016, 88.00000000000000000 ) ;
#15846 = EDGE_CURVE ( 'NONE', #10476, #5510, #20287, .T. ) ;
#15847 = DIRECTION ( 'NONE',  ( -1.000000000000000000, -0.000000000000000000, 0.000000000000000000 ) ) ;
#15848 = CARTESIAN_POINT ( 'NONE',  ( 0.000000000000000000, 0.000000000000000000, 3.000000000000000000 ) ) ;
#15849 = DIRECTION ( 'NONE',  ( -0.000000000000000000, -1.000000000000000000, -0.000000000000000000 ) ) ;
#15850 = FACE_OUTER_BOUND ( 'NONE', #4652, .T. ) ;
#15851 = DIRECTION ( 'NONE',  ( -1.000000000000000000, -0.000000000000000000, 0.000000000000000000 ) ) ;
#15852 = DIRECTION ( 'NONE',  ( 0.000000000000000000, 0.000000000000000000, 1.000000000000000000 ) ) ;
#15853 = DIRECTION ( 'NONE',  ( -1.000000000000000000, -0.000000000000000000, -0.000000000000000000 ) ) ;
#15854 = EDGE_LOOP ( 'NONE', ( #7629, #102, #4234, #7575 ) ) ;
#15855 = FACE_OUTER_BOUND ( 'NONE', #2370, .T. ) ;
#15856 = CIRCLE ( 'NONE', #2443, 32.00000000000000000 ) ;
#15857 = CIRCLE ( 'NONE', #11264, 92.50100000000000477 ) ;
#15858 = ORIENTED_EDGE ( 'NONE', *, *, #13929, .T. ) ;
#15859 = AXIS2_PLACEMENT_3D ( 'NONE', #16862, #1730, #18639 ) ;
#15860 = EDGE_CURVE ( 'NONE', #4990, #2536, #9014, .T. ) ;
#15861 = DIRECTION ( 'NONE',  ( -1.000000000000000000, 0.000000000000000000, 0.000000000000000000 ) ) ;
#15862 = EDGE_LOOP ( 'NONE', ( #1786, #11920, #1321, #14070 ) ) ;
#15863 = CYLINDRICAL_SURFACE ( 'NONE', #9854, 27.49900000000000233 ) ;
#15864 = EDGE_CURVE ( 'NONE', #10257, #12527, #12411, .T. ) ;
#15865 = DIRECTION ( 'NONE',  ( 1.000000000000000000, 0.000000000000000000, 0.000000000000000000 ) ) ;
#15866 = ORIENTED_EDGE ( 'NONE', *, *, #16707, .F. ) ;
#15867 = EDGE_CURVE ( 'NONE', #20116, #11272, #15730, .T. ) ;
#15868 = ORIENTED_EDGE ( 'NONE', *, *, #19746, .T. ) ;
#15869 = ORIENTED_EDGE ( 'NONE', *, *, #16464, .F. ) ;
#15870 = ORIENTED_EDGE ( 'NONE', *, *, #8288, .F. ) ;
#15871 = DIRECTION ( 'NONE',  ( 0.000000000000000000, -0.9510565162951503115, -0.3090169943749573322 ) ) ;
#15872 = DIRECTION ( 'NONE',  ( 1.000000000000000000, 0.000000000000000000, 0.000000000000000000 ) ) ;
#15873 = ORIENTED_EDGE ( 'NONE', *, *, #12604, .F. ) ;
#15874 = DIRECTION ( 'NONE',  ( 1.000000000000000000, 0.000000000000000000, 0.000000000000000000 ) ) ;
#15875 = DIRECTION ( 'NONE',  ( 0.000000000000000000, 0.2079116908177599532, -0.9781476007338055778 ) ) ;
#15876 = CARTESIAN_POINT ( 'NONE',  ( 10.00000000000000000, 0.000000000000000000, 0.000000000000000000 ) ) ;
#15877 = AXIS2_PLACEMENT_3D ( 'NONE', #15833, #12071, #10627 ) ;
#15878 = AXIS2_PLACEMENT_3D ( 'NONE', #8469, #9996, #6717 ) ;
#15879 = CARTESIAN_POINT ( 'NONE',  ( 10.00000000000000000, -87.92084725184945171, -3.731570516143874361 ) ) ;
#15880 = CARTESIAN_POINT ( 'NONE',  ( 0.000000000000000000, 0.000000000000000000, 5.000000000000004441 ) ) ;
#15881 = EDGE_LOOP ( 'NONE', ( #19563, #20782, #12835, #8799 ) ) ;
#15882 = CARTESIAN_POINT ( 'NONE',  ( 10.00000000000000000, 26.27606311335965827, -10.21217444509384364 ) ) ;
#15883 = DIRECTION ( 'NONE',  ( 0.000000000000000000, 0.000000000000000000, 1.000000000000000000 ) ) ;
#15884 = CARTESIAN_POINT ( 'NONE',  ( 7.599999999999998757, 105.0992000000000104, 0.000000000000000000 ) ) ;
#15885 = EDGE_LOOP ( 'NONE', ( #20777, #2974, #1239, #5267 ) ) ;
#15886 = CARTESIAN_POINT ( 'NONE',  ( 6.123233995736766282E-16, 100.0000000000000000, 5.000000000000000000 ) ) ;
#15887 = ORIENTED_EDGE ( 'NONE', *, *, #9987, .F. ) ;
#15888 = CIRCLE ( 'NONE', #11291, 1.100000000000017630 ) ;
#15889 = DIRECTION ( 'NONE',  ( -1.000000000000000000, -0.000000000000000000, -0.000000000000000000 ) ) ;
#15890 = ORIENTED_EDGE ( 'NONE', *, *, #5321, .T. ) ;
#15891 = ORIENTED_EDGE ( 'NONE', *, *, #7064, .T. ) ;
#15892 = ORIENTED_EDGE ( 'NONE', *, *, #12850, .T. ) ;
#15893 = DIRECTION ( 'NONE',  ( 0.000000000000000000, 0.000000000000000000, 1.000000000000000000 ) ) ;
#15894 = ORIENTED_EDGE ( 'NONE', *, *, #20039, .T. ) ;
#15895 = CARTESIAN_POINT ( 'NONE',  ( 10.00000000000000000, 46.89573839703386682, -79.73220629831438089 ) ) ;
#15896 = DIRECTION ( 'NONE',  ( 1.000000000000000000, 0.000000000000000000, 0.000000000000000000 ) ) ;
#15897 = DIRECTION ( 'NONE',  ( 1.000000000000000000, 0.000000000000000000, 0.000000000000000000 ) ) ;
#15898 = DIRECTION ( 'NONE',  ( 0.000000000000000000, 0.000000000000000000, 1.000000000000000000 ) ) ;
#15899 = CARTESIAN_POINT ( 'NONE',  ( 10.00000000000000000, 74.39348546125053474, 54.97312363261438151 ) ) ;
#15900 = DIRECTION ( 'NONE',  ( 0.000000000000000000, 0.000000000000000000, -1.000000000000000000 ) ) ;
#15901 = AXIS2_PLACEMENT_3D ( 'NONE', #15478, #12155, #12051 ) ;
#15902 = CARTESIAN_POINT ( 'NONE',  ( 5.000000000000000000, 51.18896083639268113, 71.57995730992199412 ) ) ;
#15903 = FACE_OUTER_BOUND ( 'NONE', #11135, .T. ) ;
#15904 = CARTESIAN_POINT ( 'NONE',  ( 9.999999999999994671, 1.276847368961009200E-14, -103.6249999999999716 ) ) ;
#15905 = ORIENTED_EDGE ( 'NONE', *, *, #15158, .T. ) ;
#15906 = VECTOR ( 'NONE', #62, 1000.000000000000000 ) ;
#15907 = EDGE_CURVE ( 'NONE', #14635, #5699, #19272, .T. ) ;
#15908 = VERTEX_POINT ( 'NONE', #20719 ) ;
#15909 = VERTEX_POINT ( 'NONE', #2253 ) ;
#15910 = VERTEX_POINT ( 'NONE', #8786 ) ;
#15911 = AXIS2_PLACEMENT_3D ( 'NONE', #16869, #5371, #10007 ) ;
#15912 = EDGE_CURVE ( 'NONE', #5806, #9874, #2151, .T. ) ;
#15913 = ORIENTED_EDGE ( 'NONE', *, *, #6236, .T. ) ;
#15914 = CYLINDRICAL_SURFACE ( 'NONE', #9109, 11.99999999999999822 ) ;
#15915 = VERTEX_POINT ( 'NONE', #12206 ) ;
#15916 = DIRECTION ( 'NONE',  ( -1.000000000000000000, -0.000000000000000000, -0.000000000000000000 ) ) ;
#15917 = DIRECTION ( 'NONE',  ( 0.000000000000000000, 0.000000000000000000, -1.000000000000000000 ) ) ;
#15918 = CARTESIAN_POINT ( 'NONE',  ( 7.599999999999998757, 0.000000000000000000, 0.000000000000000000 ) ) ;
#15919 = FACE_OUTER_BOUND ( 'NONE', #13835, .T. ) ;
#15920 = CARTESIAN_POINT ( 'NONE',  ( -1.500000000000000444, 0.000000000000000000, -5.100000000000000533 ) ) ;
#15921 = CARTESIAN_POINT ( 'NONE',  ( 0.000000000000000000, -74.39348546125016526, -54.97312363261490731 ) ) ;
#15922 = CARTESIAN_POINT ( 'NONE',  ( 0.000000000000000000, 27.48365448817206769, -0.9185515634842869037 ) ) ;
#15923 = DIRECTION ( 'NONE',  ( 0.000000000000000000, 0.000000000000000000, 1.000000000000000000 ) ) ;
#15924 = ORIENTED_EDGE ( 'NONE', *, *, #21528, .F. ) ;
#15925 = DIRECTION ( 'NONE',  ( 0.000000000000000000, 0.000000000000000000, -1.000000000000000000 ) ) ;
#15926 = ADVANCED_FACE ( 'NONE', ( #8882 ), #17191, .F. ) ;
#15927 = EDGE_CURVE ( 'NONE', #11004, #9608, #12495, .T. ) ;
#15928 = EDGE_CURVE ( 'NONE', #18327, #17060, #21379, .T. ) ;
#15929 = DIRECTION ( 'NONE',  ( 1.000000000000000000, 0.000000000000000000, 0.000000000000000000 ) ) ;
#15930 = EDGE_CURVE ( 'NONE', #20932, #3466, #2979, .T. ) ;
#15931 = CARTESIAN_POINT ( 'NONE',  ( 0.000000000000000000, -27.07404830566967746, -4.815694066514710769 ) ) ;
#15932 = ORIENTED_EDGE ( 'NONE', *, *, #18787, .F. ) ;
#15933 = CARTESIAN_POINT ( 'NONE',  ( 10.00000000000000000, 0.000000000000000000, 0.000000000000000000 ) ) ;
#15934 = ORIENTED_EDGE ( 'NONE', *, *, #670, .F. ) ;
#15935 = DIRECTION ( 'NONE',  ( 1.000000000000000000, -0.000000000000000000, 0.000000000000000000 ) ) ;
#15936 = ORIENTED_EDGE ( 'NONE', *, *, #170, .T. ) ;
#15937 = EDGE_LOOP ( 'NONE', ( #13554, #21694, #8745, #19993 ) ) ;
#15938 = CARTESIAN_POINT ( 'NONE',  ( 10.00000000000000000, 90.32141448704683739, 19.96189084378252332 ) ) ;
#15939 = DIRECTION ( 'NONE',  ( 0.000000000000000000, 0.2079116908177532919, 0.9781476007338070211 ) ) ;
#15940 = EDGE_CURVE ( 'NONE', #454, #4660, #2319, .T. ) ;
#15941 = DIRECTION ( 'NONE',  ( 0.000000000000000000, 0.000000000000000000, -1.000000000000000000 ) ) ;
#15942 = DIRECTION ( 'NONE',  ( 1.000000000000000000, 0.000000000000000000, 0.000000000000000000 ) ) ;
#15943 = DIRECTION ( 'NONE',  ( 0.000000000000000000, 0.000000000000000000, -1.000000000000000000 ) ) ;
#15944 = CYLINDRICAL_SURFACE ( 'NONE', #7555, 88.00000000000000000 ) ;
#15945 = CARTESIAN_POINT ( 'NONE',  ( 7.395800000000001262, 0.000000000000000000, -114.9007999999999896 ) ) ;
#15946 = EDGE_CURVE ( 'NONE', #2427, #21518, #15621, .T. ) ;
#15947 = CARTESIAN_POINT ( 'NONE',  ( 0.000000000000000000, 92.32475887865426500, 5.707354816230865602 ) ) ;
#15948 = CARTESIAN_POINT ( 'NONE',  ( 10.00000000000000000, -27.48365448817206058, -0.9185515634844814148 ) ) ;
#15949 = CIRCLE ( 'NONE', #5025, 0.1000000000000002554 ) ;
#15950 = EDGE_LOOP ( 'NONE', ( #7798, #5455, #11200, #2295 ) ) ;
#15951 = CARTESIAN_POINT ( 'NONE',  ( 10.00000000000000000, 0.000000000000000000, 0.000000000000000000 ) ) ;
#15952 = ORIENTED_EDGE ( 'NONE', *, *, #17435, .T. ) ;
#15953 = DIRECTION ( 'NONE',  ( -1.000000000000000000, 0.000000000000000000, -0.000000000000000000 ) ) ;
#15954 = ORIENTED_EDGE ( 'NONE', *, *, #10940, .T. ) ;
#15955 = EDGE_CURVE ( 'NONE', #10449, #17973, #11452, .T. ) ;
#15956 = DIRECTION ( 'NONE',  ( -1.000000000000000000, 0.000000000000000000, 0.000000000000000000 ) ) ;
#15957 = ORIENTED_EDGE ( 'NONE', *, *, #21116, .T. ) ;
#15958 = ORIENTED_EDGE ( 'NONE', *, *, #12871, .T. ) ;
#15959 = CIRCLE ( 'NONE', #11009, 92.50100000000000477 ) ;
#15960 = ORIENTED_EDGE ( 'NONE', *, *, #5710, .T. ) ;
#15961 = ORIENTED_EDGE ( 'NONE', *, *, #6542, .T. ) ;
#15962 = DIRECTION ( 'NONE',  ( -1.000000000000000000, 0.000000000000000000, -0.000000000000000000 ) ) ;
#15963 = CARTESIAN_POINT ( 'NONE',  ( 10.00000000000000000, 0.000000000000000000, 0.000000000000000000 ) ) ;
#15964 = VERTEX_POINT ( 'NONE', #12635 ) ;
#15965 = ADVANCED_FACE ( 'NONE', ( #17516 ), #19062, .F. ) ;
#15966 = DIRECTION ( 'NONE',  ( 0.000000000000000000, 0.000000000000000000, -1.000000000000000000 ) ) ;
#15967 = DIRECTION ( 'NONE',  ( 0.000000000000000000, 0.1391731009600657709, -0.9902680687415702510 ) ) ;
#15968 = CARTESIAN_POINT ( 'NONE',  ( 0.000000000000000000, 36.60317927562579854, 76.78148674856777234 ) ) ;
#15969 = EDGE_CURVE ( 'NONE', #20720, #14715, #17627, .T. ) ;
#15970 = DIRECTION ( 'NONE',  ( -1.000000000000000000, -0.000000000000000000, -0.000000000000000000 ) ) ;
#15971 = CARTESIAN_POINT ( 'NONE',  ( 0.000000000000000000, 28.00896854771991329, 15.47571261340933546 ) ) ;
#15972 = AXIS2_PLACEMENT_3D ( 'NONE', #19554, #10943, #7960 ) ;
#15973 = ADVANCED_FACE ( 'NONE', ( #15855 ), #717, .F. ) ;
#15974 = ORIENTED_EDGE ( 'NONE', *, *, #6, .T. ) ;
#15975 = ADVANCED_FACE ( 'NONE', ( #5798 ), #12523, .F. ) ;
#15976 = DIRECTION ( 'NONE',  ( -1.000000000000000000, -0.000000000000000000, -0.000000000000000000 ) ) ;
#15977 = CARTESIAN_POINT ( 'NONE',  ( -8.000000000000007105, 1.393954219129474843E-14, 113.8250000000000028 ) ) ;
#15978 = VECTOR ( 'NONE', #18045, 1000.000000000000000 ) ;
#15979 = CYLINDRICAL_SURFACE ( 'NONE', #3429, 12.00000000000000000 ) ;
#15980 = ORIENTED_EDGE ( 'NONE', *, *, #8114, .F. ) ;
#15981 = EDGE_CURVE ( 'NONE', #2536, #19281, #3380, .T. ) ;
#15982 = FACE_OUTER_BOUND ( 'NONE', #20963, .T. ) ;
#15983 = ORIENTED_EDGE ( 'NONE', *, *, #7599, .T. ) ;
#15984 = DIRECTION ( 'NONE',  ( 0.000000000000000000, 0.9702957262759955848, 0.2419218955996714493 ) ) ;
#15985 = ORIENTED_EDGE ( 'NONE', *, *, #10116, .T. ) ;
#15986 = ORIENTED_EDGE ( 'NONE', *, *, #5940, .F. ) ;
#15987 = ORIENTED_EDGE ( 'NONE', *, *, #5392, .T. ) ;
#15988 = CARTESIAN_POINT ( 'NONE',  ( 10.00000000000000000, 51.18896083639267403, 71.57995730992199412 ) ) ;
#15989 = ORIENTED_EDGE ( 'NONE', *, *, #15651, .T. ) ;
#15990 = DIRECTION ( 'NONE',  ( 0.000000000000000000, 0.8660254037844399289, -0.4999999999999979461 ) ) ;
#15991 = AXIS2_PLACEMENT_3D ( 'NONE', #15786, #14128, #9247 ) ;
#15992 = LINE ( 'NONE', #4284, #17113 ) ;
#15993 = CARTESIAN_POINT ( 'NONE',  ( 1.500000000000000000, 100.0000000000000000, 4.769696007084728073 ) ) ;
#15994 = DIRECTION ( 'NONE',  ( 1.000000000000000000, 0.000000000000000000, 0.000000000000000000 ) ) ;
#15995 = CIRCLE ( 'NONE', #13884, 92.50100000000003320 ) ;
#15996 = CIRCLE ( 'NONE', #1179, 88.00000000000000000 ) ;
#15997 = CARTESIAN_POINT ( 'NONE',  ( 6.123233995736766282E-16, 5.000000000000004441, 5.000000000000000000 ) ) ;
#15998 = DIRECTION ( 'NONE',  ( 0.000000000000000000, 0.000000000000000000, -1.000000000000000000 ) ) ;
#15999 = DIRECTION ( 'NONE',  ( -1.000000000000000000, -0.000000000000000000, 0.000000000000000000 ) ) ;
#16000 = CARTESIAN_POINT ( 'NONE',  ( 5.000000000000000000, -65.83713140174687339, -58.39068529131263574 ) ) ;
#16001 = DIRECTION ( 'NONE',  ( -1.000000000000000000, -0.000000000000000000, -0.000000000000000000 ) ) ;
#16002 = AXIS2_PLACEMENT_3D ( 'NONE', #7692, #15970, #836 ) ;
#16003 = CARTESIAN_POINT ( 'NONE',  ( 10.00000000000000000, 15.51843147776349063, 83.63233659819657362 ) ) ;
#16004 = CIRCLE ( 'NONE', #16716, 88.00000000000000000 ) ;
#16005 = ORIENTED_EDGE ( 'NONE', *, *, #10940, .F. ) ;
#16006 = ORIENTED_EDGE ( 'NONE', *, *, #14454, .F. ) ;
#16007 = VECTOR ( 'NONE', #17971, 1000.000000000000000 ) ;
#16008 = ORIENTED_EDGE ( 'NONE', *, *, #15255, .T. ) ;
#16009 = ORIENTED_EDGE ( 'NONE', *, *, #18697, .F. ) ;
#16010 = VERTEX_POINT ( 'NONE', #12852 ) ;
#16011 = DIRECTION ( 'NONE',  ( 0.000000000000000000, -0.8660254037844328234, -0.5000000000000101030 ) ) ;
#16012 = AXIS2_PLACEMENT_3D ( 'NONE', #168, #15517, #10318 ) ;
#16013 = ORIENTED_EDGE ( 'NONE', *, *, #4326, .T. ) ;
#16014 = DIRECTION ( 'NONE',  ( 1.000000000000000000, 0.000000000000000000, 0.000000000000000000 ) ) ;
#16015 = DIRECTION ( 'NONE',  ( 0.000000000000000000, -1.603655480014115143E-14, -1.000000000000000000 ) ) ;
#16016 = DIRECTION ( 'NONE',  ( -1.000000000000000000, 0.000000000000000000, 0.000000000000000000 ) ) ;
#16017 = AXIS2_PLACEMENT_3D ( 'NONE', #8585, #12110, #13668 ) ;
#16018 = CARTESIAN_POINT ( 'NONE',  ( 10.00000000000000000, 41.87002153499211232, -74.04114219178001122 ) ) ;
#16019 = CARTESIAN_POINT ( 'NONE',  ( 10.00000000000000000, -16.79755869217711250, 90.96305306542248559 ) ) ;
#16020 = EDGE_CURVE ( 'NONE', #17231, #15586, #10076, .T. ) ;
#16021 = DIRECTION ( 'NONE',  ( 0.000000000000000000, 0.2079116908177532919, 0.9781476007338070211 ) ) ;
#16022 = AXIS2_PLACEMENT_3D ( 'NONE', #6117, #14831, #11075 ) ;
#16023 = CARTESIAN_POINT ( 'NONE',  ( 10.00000000000000000, 0.000000000000000000, 0.000000000000000000 ) ) ;
#16024 = CARTESIAN_POINT ( 'NONE',  ( -10.00000000000000000, 0.000000000000000000, 0.000000000000000000 ) ) ;
#16025 = DIRECTION ( 'NONE',  ( 1.000000000000000000, 0.000000000000000000, 0.000000000000000000 ) ) ;
#16026 = VERTEX_POINT ( 'NONE', #6131 ) ;
#16027 = EDGE_CURVE ( 'NONE', #16206, #16668, #18220, .T. ) ;
#16028 = CARTESIAN_POINT ( 'NONE',  ( 10.00000000000000000, -87.17509410653602231, -30.93441398372672069 ) ) ;
#16029 = AXIS2_PLACEMENT_3D ( 'NONE', #6859, #228, #12954 ) ;
#16030 = CIRCLE ( 'NONE', #19924, 118.9000000000000199 ) ;
#16031 = TOROIDAL_SURFACE ( 'NONE', #10389, 7.400000000000020783, 0.1000000000000001582 ) ;
#16032 = FACE_OUTER_BOUND ( 'NONE', #15147, .T. ) ;
#16033 = AXIS2_PLACEMENT_3D ( 'NONE', #3690, #17066, #1923 ) ;
#16034 = CYLINDRICAL_SURFACE ( 'NONE', #8838, 12.00000000000000000 ) ;
#16035 = ORIENTED_EDGE ( 'NONE', *, *, #7314, .T. ) ;
#16036 = CARTESIAN_POINT ( 'NONE',  ( 10.00000000000000000, -7.619321854369379032, -26.42235673590698397 ) ) ;
#16037 = ORIENTED_EDGE ( 'NONE', *, *, #13285, .F. ) ;
#16038 = ORIENTED_EDGE ( 'NONE', *, *, #6796, .F. ) ;
#16039 = VECTOR ( 'NONE', #16555, 1000.000000000000000 ) ;
#16040 = CARTESIAN_POINT ( 'NONE',  ( 10.00000000000000000, 0.000000000000000000, 0.000000000000000000 ) ) ;
#16041 = VERTEX_POINT ( 'NONE', #9531 ) ;
#16042 = ORIENTED_EDGE ( 'NONE', *, *, #20383, .T. ) ;
#16043 = DIRECTION ( 'NONE',  ( -1.000000000000000000, 0.000000000000000000, -0.000000000000000000 ) ) ;
#16044 = CARTESIAN_POINT ( 'NONE',  ( 10.00000000000000000, 87.44637528609675314, -9.855528870797693131 ) ) ;
#16045 = CIRCLE ( 'NONE', #19227, 32.00000000000000000 ) ;
#16046 = DIRECTION ( 'NONE',  ( -1.000000000000000000, -0.000000000000000000, -0.000000000000000000 ) ) ;
#16047 = CARTESIAN_POINT ( 'NONE',  ( 5.000000000000000888, -31.75612719289743779, 3.943144139962448058 ) ) ;
#16048 = EDGE_CURVE ( 'NONE', #20174, #9814, #16060, .T. ) ;
#16050 = EDGE_CURVE ( 'NONE', #17052, #16573, #16177, .T. ) ;
#16049 = CIRCLE ( 'NONE', #8659, 92.50100000000000477 ) ;
#16051 = DIRECTION ( 'NONE',  ( -1.000000000000000000, 0.000000000000000000, -0.000000000000000000 ) ) ;
#16052 = DIRECTION ( 'NONE',  ( -1.000000000000000000, -0.000000000000000000, 0.000000000000000000 ) ) ;
#16053 = TOROIDAL_SURFACE ( 'NONE', #21705, 5.633200000000004870, 0.02570000000000143697 ) ;
#16054 = CARTESIAN_POINT ( 'NONE',  ( -123.5000000000000142, 1.512438796946981289E-14, 0.000000000000000000 ) ) ;
#16055 = CARTESIAN_POINT ( 'NONE',  ( 5.000000000000002665, -81.83745710415254848, -32.35167097270233683 ) ) ;
#16057 = CIRCLE ( 'NONE', #6896, 120.0000000000000000 ) ;
#16056 = LINE ( 'NONE', #14404, #17204 ) ;
#16058 = ORIENTED_EDGE ( 'NONE', *, *, #1528, .F. ) ;
#16059 = AXIS2_PLACEMENT_3D ( 'NONE', #1740, #15316, #5173 ) ;
#16060 = LINE ( 'NONE', #7786, #4092 ) ;
#16061 = VERTEX_POINT ( 'NONE', #17841 ) ;
#16062 = AXIS2_PLACEMENT_3D ( 'NONE', #10215, #8662, #5463 ) ;
#16063 = CARTESIAN_POINT ( 'NONE',  ( 0.000000000000000000, -28.15804365424196121, 10.64184787299373269 ) ) ;
#16064 = EDGE_CURVE ( 'NONE', #11402, #1182, #4467, .T. ) ;
#16065 = DIRECTION ( 'NONE',  ( 0.000000000000000000, -0.1391731009600517543, -0.9902680687415721383 ) ) ;
#16066 = CIRCLE ( 'NONE', #12550, 44.99999999999999289 ) ;
#16067 = CYLINDRICAL_SURFACE ( 'NONE', #1401, 92.50100000000000477 ) ;
#16068 = CIRCLE ( 'NONE', #4789, 11.99999999999999822 ) ;
#16069 = ORIENTED_EDGE ( 'NONE', *, *, #20574, .T. ) ;
#16070 = AXIS2_PLACEMENT_3D ( 'NONE', #14965, #3257, #16410 ) ;
#16071 = EDGE_CURVE ( 'NONE', #13874, #13666, #10440, .T. ) ;
#16072 = VECTOR ( 'NONE', #20576, 1000.000000000000000 ) ;
#16073 = ORIENTED_EDGE ( 'NONE', *, *, #16472, .T. ) ;
#16074 = ORIENTED_EDGE ( 'NONE', *, *, #18512, .F. ) ;
#16075 = EDGE_LOOP ( 'NONE', ( #7739, #7491 ) ) ;
#16076 = CARTESIAN_POINT ( 'NONE',  ( 0.000000000000000000, 88.70892494636740366, 26.21376805916615282 ) ) ;
#16077 = FACE_OUTER_BOUND ( 'NONE', #766, .T. ) ;
#16078 = ORIENTED_EDGE ( 'NONE', *, *, #9308, .F. ) ;
#16079 = EDGE_CURVE ( 'NONE', #11398, #10855, #17730, .T. ) ;
#16080 = DIRECTION ( 'NONE',  ( 0.000000000000000000, 0.000000000000000000, -1.000000000000000000 ) ) ;
#16081 = EDGE_CURVE ( 'NONE', #8553, #11931, #11203, .T. ) ;
#16082 = PLANE ( 'NONE',  #16772 ) ;
#16083 = ADVANCED_FACE ( 'NONE', ( #21370 ), #12745, .F. ) ;
#16084 = CARTESIAN_POINT ( 'NONE',  ( 10.00000000000000000, 17.83210509884670714, -21.83428559348744002 ) ) ;
#16085 = CIRCLE ( 'NONE', #17864, 88.00000000000000000 ) ;
#16086 = CARTESIAN_POINT ( 'NONE',  ( 10.00000000000000000, -92.22057093985026199, -7.197311757041478408 ) ) ;
#16087 = ADVANCED_FACE ( 'NONE', ( #1042 ), #21260, .F. ) ;
#16088 = AXIS2_PLACEMENT_3D ( 'NONE', #20017, #13592, #3437 ) ;
#16089 = ORIENTED_EDGE ( 'NONE', *, *, #6678, .F. ) ;
#16090 = AXIS2_PLACEMENT_3D ( 'NONE', #2687, #803, #7449 ) ;
#16091 = DIRECTION ( 'NONE',  ( -1.000000000000000000, -0.000000000000000000, -0.000000000000000000 ) ) ;
#16092 = CIRCLE ( 'NONE', #8983, 44.99999999999998579 ) ;
#16093 = DIRECTION ( 'NONE',  ( 0.000000000000000000, 0.000000000000000000, -1.000000000000000000 ) ) ;
#16094 = DIRECTION ( 'NONE',  ( -1.000000000000000000, -0.000000000000000000, -0.000000000000000000 ) ) ;
#16095 = ADVANCED_FACE ( 'NONE', ( #17688 ), #20886, .F. ) ;
#16096 = ORIENTED_EDGE ( 'NONE', *, *, #3234, .F. ) ;
#16097 = CARTESIAN_POINT ( 'NONE',  ( 10.00000000000000000, -88.70892494636720471, -26.21376805916674613 ) ) ;
#16098 = ORIENTED_EDGE ( 'NONE', *, *, #5125, .F. ) ;
#16099 = DIRECTION ( 'NONE',  ( 1.000000000000000000, 0.000000000000000000, 0.000000000000000000 ) ) ;
#16100 = EDGE_CURVE ( 'NONE', #16815, #15166, #10722, .T. ) ;
#16101 = ORIENTED_EDGE ( 'NONE', *, *, #5166, .F. ) ;
#16102 = VERTEX_POINT ( 'NONE', #17261 ) ;
#16103 = AXIS2_PLACEMENT_3D ( 'NONE', #13239, #4853, #9693 ) ;
#16104 = VERTEX_POINT ( 'NONE', #17585 ) ;
#16105 = CARTESIAN_POINT ( 'NONE',  ( 10.00000000000000000, -33.95793648385753727, -86.04239391578025220 ) ) ;
#16106 = CIRCLE ( 'NONE', #6601, 27.49900000000000588 ) ;
#16107 = EDGE_CURVE ( 'NONE', #453, #6547, #6930, .T. ) ;
#16108 = ORIENTED_EDGE ( 'NONE', *, *, #7209, .T. ) ;
#16109 = DIRECTION ( 'NONE',  ( 1.000000000000000000, -0.000000000000000000, 0.000000000000000000 ) ) ;
#16110 = CARTESIAN_POINT ( 'NONE',  ( 7.999999999999979572, 0.000000000000000000, -113.8250000000000171 ) ) ;
#16111 = DIRECTION ( 'NONE',  ( -1.000000000000000000, -0.000000000000000000, -0.000000000000000000 ) ) ;
#16112 = CARTESIAN_POINT ( 'NONE',  ( 0.000000000000000000, 27.00677879429026618, 80.65868421664441712 ) ) ;
#16113 = ADVANCED_FACE ( 'NONE', ( #677 ), #19344, .F. ) ;
#16114 = FACE_OUTER_BOUND ( 'NONE', #7259, .T. ) ;
#16115 = CARTESIAN_POINT ( 'NONE',  ( 10.00000000000000000, -47.19205848891713373, -74.27590198428171675 ) ) ;
#16116 = CARTESIAN_POINT ( 'NONE',  ( 0.000000000000000000, 75.87763420127832603, 44.57111876559751096 ) ) ;
#16117 = CARTESIAN_POINT ( 'NONE',  ( -90.00000000000000000, 0.000000000000000000, 0.000000000000000000 ) ) ;
#16118 = CIRCLE ( 'NONE', #17899, 92.50100000000000477 ) ;
#16119 = CIRCLE ( 'NONE', #631, 5.612499999999999822 ) ;
#16120 = CIRCLE ( 'NONE', #17534, 92.50100000000000477 ) ;
#16121 = CIRCLE ( 'NONE', #10128, 92.50100000000000477 ) ;
#16122 = CARTESIAN_POINT ( 'NONE',  ( 0.000000000000000000, -18.94217447942616417, 85.93715160505946926 ) ) ;
#16123 = ORIENTED_EDGE ( 'NONE', *, *, #10115, .F. ) ;
#16124 = ORIENTED_EDGE ( 'NONE', *, *, #1642, .T. ) ;
#16125 = EDGE_CURVE ( 'NONE', #20835, #7559, #9719, .T. ) ;
#16126 = VERTEX_POINT ( 'NONE', #5875 ) ;
#16127 = ORIENTED_EDGE ( 'NONE', *, *, #702, .T. ) ;
#16128 = EDGE_CURVE ( 'NONE', #19694, #20854, #2441, .T. ) ;
#16129 = ORIENTED_EDGE ( 'NONE', *, *, #7432, .F. ) ;
#16130 = DIRECTION ( 'NONE',  ( 1.000000000000000000, 0.000000000000000000, 0.000000000000000000 ) ) ;
#16131 = AXIS2_PLACEMENT_3D ( 'NONE', #15755, #4262, #12868 ) ;
#16132 = EDGE_LOOP ( 'NONE', ( #10322, #8501, #12917, #4827 ) ) ;
#16133 = DIRECTION ( 'NONE',  ( 0.000000000000000000, -0.6946583704590034714, 0.7193398003386453077 ) ) ;
#16134 = AXIS2_PLACEMENT_3D ( 'NONE', #6280, #11565, #1502 ) ;
#16135 = FACE_BOUND ( 'NONE', #6257, .T. ) ;
#16136 = AXIS2_PLACEMENT_3D ( 'NONE', #13228, #9475, #7825 ) ;
#16137 = DIRECTION ( 'NONE',  ( 1.000000000000000000, 0.000000000000000000, 0.000000000000000000 ) ) ;
#16138 = DIRECTION ( 'NONE',  ( 0.000000000000000000, -0.9510565162951503115, -0.3090169943749573878 ) ) ;
#16139 = DIRECTION ( 'NONE',  ( -1.000000000000000000, 0.000000000000000000, -0.000000000000000000 ) ) ;
#16140 = DIRECTION ( 'NONE',  ( 1.000000000000000000, -0.000000000000000000, -0.000000000000000000 ) ) ;
#16141 = CARTESIAN_POINT ( 'NONE',  ( 0.000000000000000000, 12.90282758292980247, 25.06465718894781247 ) ) ;
#16142 = CARTESIAN_POINT ( 'NONE',  ( -10.00000000000000000, 0.000000000000000000, 0.000000000000000000 ) ) ;
#16143 = DIRECTION ( 'NONE',  ( -1.000000000000000000, 0.000000000000000000, 0.000000000000000000 ) ) ;
#16144 = ORIENTED_EDGE ( 'NONE', *, *, #6354, .T. ) ;
#16145 = DIRECTION ( 'NONE',  ( -1.000000000000000000, -0.000000000000000000, -0.000000000000000000 ) ) ;
#16146 = AXIS2_PLACEMENT_3D ( 'NONE', #17745, #5703, #2595 ) ;
#16147 = AXIS2_PLACEMENT_3D ( 'NONE', #21708, #8233, #8134 ) ;
#16148 = ORIENTED_EDGE ( 'NONE', *, *, #8529, .T. ) ;
#16149 = CIRCLE ( 'NONE', #5233, 27.49900000000000588 ) ;
#16150 = EDGE_CURVE ( 'NONE', #5864, #16720, #6874, .T. ) ;
#16151 = DIRECTION ( 'NONE',  ( -1.000000000000000000, -0.000000000000000000, 0.000000000000000000 ) ) ;
#16152 = DIRECTION ( 'NONE',  ( 1.000000000000000000, 0.000000000000000000, 0.000000000000000000 ) ) ;
#16153 = VERTEX_POINT ( 'NONE', #12273 ) ;
#16154 = CYLINDRICAL_SURFACE ( 'NONE', #13596, 10.49999999999999822 ) ;
#16155 = VERTEX_POINT ( 'NONE', #15700 ) ;
#16156 = VERTEX_POINT ( 'NONE', #14042 ) ;
#16157 = DIRECTION ( 'NONE',  ( 2.140611735271806545E-17, 1.000000000000000000, 4.506460675456325137E-17 ) ) ;
#16158 = AXIS2_PLACEMENT_3D ( 'NONE', #8636, #20683, #5546 ) ;
#16159 = DIRECTION ( 'NONE',  ( -1.000000000000000000, -0.000000000000000000, -0.000000000000000000 ) ) ;
#16160 = ORIENTED_EDGE ( 'NONE', *, *, #15981, .T. ) ;
#16161 = VERTEX_POINT ( 'NONE', #17478 ) ;
#16162 = FACE_OUTER_BOUND ( 'NONE', #8066, .T. ) ;
#16163 = CARTESIAN_POINT ( 'NONE',  ( 10.00000000000000000, -23.57863763525731216, 15.45211464167656601 ) ) ;
#16164 = AXIS2_PLACEMENT_3D ( 'NONE', #356, #13931, #20673 ) ;
#16165 = AXIS2_PLACEMENT_3D ( 'NONE', #15848, #12512, #15942 ) ;
#16166 = DIRECTION ( 'NONE',  ( 0.000000000000000000, 0.000000000000000000, 1.000000000000000000 ) ) ;
#16167 = CARTESIAN_POINT ( 'NONE',  ( 0.000000000000000000, -27.48365448817206058, -0.9185515634844814148 ) ) ;
#16168 = VECTOR ( 'NONE', #474, 1000.000000000000000 ) ;
#16169 = CARTESIAN_POINT ( 'NONE',  ( 0.000000000000000000, 0.000000000000000000, 0.000000000000000000 ) ) ;
#16170 = CIRCLE ( 'NONE', #5248, 27.49900000000000233 ) ;
#16171 = DIRECTION ( 'NONE',  ( 1.000000000000000000, 0.000000000000000000, 0.000000000000000000 ) ) ;
#16172 = VECTOR ( 'NONE', #346, 1000.000000000000000 ) ;
#16173 = DIRECTION ( 'NONE',  ( 0.000000000000000000, 0.000000000000000000, 1.000000000000000000 ) ) ;
#16174 = DIRECTION ( 'NONE',  ( -1.000000000000000000, 0.000000000000000000, 0.000000000000000000 ) ) ;
#16175 = CARTESIAN_POINT ( 'NONE',  ( 1.500000000000000000, -4.769696007084728073, 15.00000000000000000 ) ) ;
#16176 = ORIENTED_EDGE ( 'NONE', *, *, #452, .T. ) ;
#16177 = LINE ( 'NONE', #924, #7268 ) ;
#16178 = ORIENTED_EDGE ( 'NONE', *, *, #19673, .F. ) ;
#16179 = DIRECTION ( 'NONE',  ( 1.000000000000000000, 0.000000000000000000, 0.000000000000000000 ) ) ;
#16180 = AXIS2_PLACEMENT_3D ( 'NONE', #18454, #8286, #14910 ) ;
#16181 = FILL_AREA_STYLE_COLOUR ( '', #13406 ) ;
#16182 = EDGE_CURVE ( 'NONE', #286, #1246, #7570, .T. ) ;
#16183 = AXIS2_PLACEMENT_3D ( 'NONE', #18144, #1860, #3304 ) ;
#16184 = AXIS2_PLACEMENT_3D ( 'NONE', #19413, #12769, #6167 ) ;
#16185 = DIRECTION ( 'NONE',  ( 1.000000000000000000, 0.000000000000000000, 0.000000000000000000 ) ) ;
#16186 = AXIS2_PLACEMENT_3D ( 'NONE', #4408, #6186, #6518 ) ;
#16187 = ORIENTED_EDGE ( 'NONE', *, *, #12306, .T. ) ;
#16188 = ORIENTED_EDGE ( 'NONE', *, *, #2748, .T. ) ;
#16189 = ORIENTED_EDGE ( 'NONE', *, *, #19619, .T. ) ;
#16190 = ORIENTED_EDGE ( 'NONE', *, *, #17489, .F. ) ;
#16191 = DIRECTION ( 'NONE',  ( 1.000000000000000000, 0.000000000000000000, 0.000000000000000000 ) ) ;
#16192 = CARTESIAN_POINT ( 'NONE',  ( 10.00000000000000000, 26.69209308833516658, -6.612652082459054448 ) ) ;
#16193 = EDGE_CURVE ( 'NONE', #21294, #4861, #3986, .T. ) ;
#16194 = ORIENTED_EDGE ( 'NONE', *, *, #288, .T. ) ;
#16195 = CARTESIAN_POINT ( 'NONE',  ( -120.0000000000000000, 1.469576158976823671E-14, 25.00000000000000000 ) ) ;
#16196 = DIRECTION ( 'NONE',  ( 0.000000000000000000, 0.000000000000000000, 1.000000000000000000 ) ) ;
#16197 = CARTESIAN_POINT ( 'NONE',  ( 0.000000000000000000, -25.56104204395249369, -81.12843256239690959 ) ) ;
#16198 = DIRECTION ( 'NONE',  ( 0.000000000000000000, -0.8290375725550467312, 0.5591929034707392443 ) ) ;
#16199 = DIRECTION ( 'NONE',  ( 1.000000000000000000, -0.000000000000000000, -0.000000000000000000 ) ) ;
#16200 = EDGE_CURVE ( 'NONE', #13661, #13981, #9324, .T. ) ;
#16201 = AXIS2_PLACEMENT_3D ( 'NONE', #9522, #9738, #13063 ) ;
#16202 = CONICAL_SURFACE ( 'NONE', #3491, 5.453125000000000000, 0.4883339510564123076 ) ;
#16203 = VERTEX_POINT ( 'NONE', #17364 ) ;
#16204 = DIRECTION ( 'NONE',  ( 0.000000000000000000, -0.06975647374411138302, -0.9975640502598251969 ) ) ;
#16205 = CARTESIAN_POINT ( 'NONE',  ( 10.00000000000000000, -12.90282758292996235, 25.06465718894773431 ) ) ;
#16206 = VERTEX_POINT ( 'NONE', #4101 ) ;
#16207 = DIRECTION ( 'NONE',  ( -1.000000000000000000, -0.000000000000000000, -0.000000000000000000 ) ) ;
#16208 = ORIENTED_EDGE ( 'NONE', *, *, #18772, .F. ) ;
#16209 = EDGE_CURVE ( 'NONE', #826, #4912, #18875, .T. ) ;
#16210 = DIRECTION ( 'NONE',  ( -0.000000000000000000, 1.000000000000000000, 0.000000000000000000 ) ) ;
#16211 = EDGE_CURVE ( 'NONE', #21386, #1889, #15341, .T. ) ;
#16212 = EDGE_CURVE ( 'NONE', #16041, #16573, #2994, .T. ) ;
#16213 = DIRECTION ( 'NONE',  ( 0.000000000000000000, -0.5877852522924797984, 0.8090169943749424553 ) ) ;
#16214 = ORIENTED_EDGE ( 'NONE', *, *, #6102, .F. ) ;
#16215 = CYLINDRICAL_SURFACE ( 'NONE', #6039, 44.99999999999999289 ) ;
#16216 = EDGE_CURVE ( 'NONE', #18291, #7130, #2282, .T. ) ;
#16217 = VERTEX_POINT ( 'NONE', #884 ) ;
#16218 = VERTEX_POINT ( 'NONE', #7633 ) ;
#16219 = ORIENTED_EDGE ( 'NONE', *, *, #19892, .T. ) ;
#16220 = CIRCLE ( 'NONE', #9142, 92.50099999999999056 ) ;
#16221 = DIRECTION ( 'NONE',  ( -1.000000000000000000, -0.000000000000000000, -0.000000000000000000 ) ) ;
#16222 = AXIS2_PLACEMENT_3D ( 'NONE', #14650, #3165, #16204 ) ;
#16223 = VERTEX_POINT ( 'NONE', #15813 ) ;
#16224 = DIRECTION ( 'NONE',  ( 0.000000000000000000, 0.000000000000000000, 1.000000000000000000 ) ) ;
#16225 = CARTESIAN_POINT ( 'NONE',  ( 0.000000000000000000, -1.959304526717989381, 27.42911093658674559 ) ) ;
#16226 = DIRECTION ( 'NONE',  ( 0.000000000000000000, -0.5877852522924632561, -0.8090169943749545567 ) ) ;
#16227 = CARTESIAN_POINT ( 'NONE',  ( -8.900000000000019895, 0.000000000000000000, -100.0000000000000284 ) ) ;
#16228 = EDGE_CURVE ( 'NONE', #6035, #16620, #14637, .T. ) ;
#16229 = DIRECTION ( 'NONE',  ( -1.000000000000000000, -0.000000000000000000, -0.000000000000000000 ) ) ;
#16230 = DIRECTION ( 'NONE',  ( 0.000000000000000000, 0.000000000000000000, 1.000000000000000000 ) ) ;
#16231 = DIRECTION ( 'NONE',  ( -1.000000000000000000, -0.000000000000000000, -0.000000000000000000 ) ) ;
#16232 = ADVANCED_FACE ( 'NONE', ( #19447 ), #570, .F. ) ;
#16233 = FACE_OUTER_BOUND ( 'NONE', #190, .T. ) ;
#16234 = AXIS2_PLACEMENT_3D ( 'NONE', #6367, #9535, #13076 ) ;
#16235 = CARTESIAN_POINT ( 'NONE',  ( 10.00000000000000000, 0.000000000000000000, 0.000000000000000000 ) ) ;
#16236 = ORIENTED_EDGE ( 'NONE', *, *, #3830, .T. ) ;
#16237 = ORIENTED_EDGE ( 'NONE', *, *, #2208, .F. ) ;
#16238 = ORIENTED_EDGE ( 'NONE', *, *, #18418, .F. ) ;
#16239 = ADVANCED_FACE ( 'NONE', ( #18554 ), #18342, .T. ) ;
#16240 = VERTEX_POINT ( 'NONE', #15007 ) ;
#16241 = ORIENTED_EDGE ( 'NONE', *, *, #7879, .F. ) ;
#16242 = CARTESIAN_POINT ( 'NONE',  ( 10.00000000000000000, 10.41137886060228901, -91.91321010181836471 ) ) ;
#16243 = ORIENTED_EDGE ( 'NONE', *, *, #12879, .F. ) ;
#16244 = CYLINDRICAL_SURFACE ( 'NONE', #5373, 88.00000000000000000 ) ;
#16245 = AXIS2_PLACEMENT_3D ( 'NONE', #4322, #1020, #2790 ) ;
#16246 = CARTESIAN_POINT ( 'NONE',  ( 0.000000000000000000, -0.6609040254605957898, -87.99751818016876825 ) ) ;
#16247 = EDGE_CURVE ( 'NONE', #5584, #5601, #4403, .T. ) ;
#16248 = DIRECTION ( 'NONE',  ( 0.000000000000000000, 0.000000000000000000, -1.000000000000000000 ) ) ;
#16249 = CARTESIAN_POINT ( 'NONE',  ( 5.000000000000002665, -18.94217447942616417, 85.93715160505946926 ) ) ;
#16250 = DIRECTION ( 'NONE',  ( 0.000000000000000000, 0.9510565162951523099, 0.3090169943749512815 ) ) ;
#16251 = EDGE_CURVE ( 'NONE', #14961, #11159, #6892, .T. ) ;
#16252 = DIRECTION ( 'NONE',  ( -1.000000000000000000, 0.000000000000000000, 0.000000000000000000 ) ) ;
#16253 = DIRECTION ( 'NONE',  ( -1.000000000000000000, 0.000000000000000000, 0.000000000000000000 ) ) ;
#16254 = DIRECTION ( 'NONE',  ( -1.000000000000000000, -0.000000000000000000, -0.000000000000000000 ) ) ;
#16255 = EDGE_CURVE ( 'NONE', #1245, #2769, #16030, .T. ) ;
#16256 = ORIENTED_EDGE ( 'NONE', *, *, #17886, .F. ) ;
#16257 = ADVANCED_FACE ( 'NONE', ( #20204 ), #13025, .T. ) ;
#16258 = DIRECTION ( 'NONE',  ( 0.000000000000000000, -0.2079116908177664480, 0.9781476007338041345 ) ) ;
#16259 = VECTOR ( 'NONE', #18701, 1000.000000000000000 ) ;
#16260 = VERTEX_POINT ( 'NONE', #2966 ) ;
#16261 = CARTESIAN_POINT ( 'NONE',  ( 10.00000000000000000, 3.786343810537937227, -27.23708136986048700 ) ) ;
#16262 = DIRECTION ( 'NONE',  ( -1.000000000000000000, 0.000000000000000000, 0.000000000000000000 ) ) ;
#16263 = EDGE_LOOP ( 'NONE', ( #3892, #14222, #2341, #14392 ) ) ;
#16264 = DIRECTION ( 'NONE',  ( -1.000000000000000000, 0.000000000000000000, 0.000000000000000000 ) ) ;
#16265 = ORIENTED_EDGE ( 'NONE', *, *, #19619, .F. ) ;
#16266 = VERTEX_POINT ( 'NONE', #3190 ) ;
#16267 = DIRECTION ( 'NONE',  ( 1.000000000000000000, -0.000000000000000000, 0.000000000000000000 ) ) ;
#16268 = ORIENTED_EDGE ( 'NONE', *, *, #21246, .T. ) ;
#16269 = ORIENTED_EDGE ( 'NONE', *, *, #13237, .T. ) ;
#16270 = DIRECTION ( 'NONE',  ( 1.000000000000000000, 0.000000000000000000, 0.000000000000000000 ) ) ;
#16271 = CYLINDRICAL_SURFACE ( 'NONE', #6715, 12.00000000000000000 ) ;
#16272 = DIRECTION ( 'NONE',  ( 1.000000000000000000, -0.000000000000000000, -0.000000000000000000 ) ) ;
#16273 = DIRECTION ( 'NONE',  ( 0.000000000000000000, 0.000000000000000000, 1.000000000000000000 ) ) ;
#16274 = COLOUR_RGB ( '', 0.31764706, 0.68627451, 0.89019608) ;
#16275 = LINE ( 'NONE', #20224, #9667 ) ;
#16276 = DIRECTION ( 'NONE',  ( -1.000000000000000000, -0.000000000000000000, -0.000000000000000000 ) ) ;
#16277 = CARTESIAN_POINT ( 'NONE',  ( 10.00000000000000000, 0.000000000000000000, 0.000000000000000000 ) ) ;
#16278 = CYLINDRICAL_SURFACE ( 'NONE', #8060, 88.00000000000000000 ) ;
#16279 = ORIENTED_EDGE ( 'NONE', *, *, #21847, .F. ) ;
#16280 = CARTESIAN_POINT ( 'NONE',  ( -10.00000000000000000, 0.000000000000000000, 0.000000000000000000 ) ) ;
#16281 = ORIENTED_EDGE ( 'NONE', *, *, #17299, .F. ) ;
#16282 = CARTESIAN_POINT ( 'NONE',  ( 10.00000000000000000, 86.54587337002878655, 15.93147207947034971 ) ) ;
#16283 = AXIS2_PLACEMENT_3D ( 'NONE', #1129, #11295, #7656 ) ;
#16284 = FACE_OUTER_BOUND ( 'NONE', #20308, .T. ) ;
#16285 = EDGE_LOOP ( 'NONE', ( #17313, #21259, #12030, #8736 ) ) ;
#16286 =( NAMED_UNIT ( * ) PLANE_ANGLE_UNIT ( ) SI_UNIT ( $, .RADIAN. ) );
#16287 = ORIENTED_EDGE ( 'NONE', *, *, #16829, .T. ) ;
#16288 = ORIENTED_EDGE ( 'NONE', *, *, #14777, .T. ) ;
#16289 = ORIENTED_EDGE ( 'NONE', *, *, #19314, .F. ) ;
#16290 = DIRECTION ( 'NONE',  ( 1.000000000000000000, -0.000000000000000000, -0.000000000000000000 ) ) ;
#16291 = ORIENTED_EDGE ( 'NONE', *, *, #5342, .F. ) ;
#16292 = ORIENTED_EDGE ( 'NONE', *, *, #18059, .F. ) ;
#16293 = AXIS2_PLACEMENT_3D ( 'NONE', #12782, #755, #7498 ) ;
#16294 = CARTESIAN_POINT ( 'NONE',  ( 10.00000000000000000, 0.000000000000000000, 0.000000000000000000 ) ) ;
#16295 = CARTESIAN_POINT ( 'NONE',  ( 10.00000000000000000, -52.34334029047928993, 76.26670130689468863 ) ) ;
#16296 = CARTESIAN_POINT ( 'NONE',  ( 1.139999999999995017, 0.000000000000000000, -5.633200000000004870 ) ) ;
#16297 = DIRECTION ( 'NONE',  ( 0.000000000000000000, 0.6946583704589983643, -0.7193398003386500816 ) ) ;
#16298 = DIRECTION ( 'NONE',  ( -1.000000000000000000, -0.000000000000000000, -0.000000000000000000 ) ) ;
#16299 = UNCERTAINTY_MEASURE_WITH_UNIT (LENGTH_MEASURE( 1.000000000000000082E-05 ), #16383, 'distance_accuracy_value', 'NONE');
#16300 = ADVANCED_FACE ( 'NONE', ( #19871 ), #14799, .T. ) ;
#16301 = PRODUCT_DEFINITION_FORMATION_WITH_SPECIFIED_SOURCE ( 'ANY', '', #8086, .NOT_KNOWN. ) ;
#16302 = VERTEX_POINT ( 'NONE', #1526 ) ;
#16303 = CARTESIAN_POINT ( 'NONE',  ( 0.000000000000000000, 0.000000000000000000, 0.000000000000000000 ) ) ;
#16304 = CIRCLE ( 'NONE', #15241, 11.99999999999999822 ) ;
#16305 = DIRECTION ( 'NONE',  ( -1.000000000000000000, 0.000000000000000000, -0.000000000000000000 ) ) ;
#16306 = VERTEX_POINT ( 'NONE', #19472 ) ;
#16307 = EDGE_CURVE ( 'NONE', #3827, #16396, #21539, .T. ) ;
#16308 = CARTESIAN_POINT ( 'NONE',  ( 10.00000000000000000, -56.05743251323810483, -67.83483072893858434 ) ) ;
#16309 = EDGE_LOOP ( 'NONE', ( #1779, #7951, #8631, #11808 ) ) ;
#16310 = VECTOR ( 'NONE', #5355, 1000.000000000000000 ) ;
#16311 = DIRECTION ( 'NONE',  ( -1.000000000000000000, -0.000000000000000000, -0.000000000000000000 ) ) ;
#16312 = CARTESIAN_POINT ( 'NONE',  ( 0.000000000000000000, 84.12297548659721258, -12.59025161327029529 ) ) ;
#16313 = ORIENTED_EDGE ( 'NONE', *, *, #209, .T. ) ;
#16314 = AXIS2_PLACEMENT_3D ( 'NONE', #206, #5290, #17101 ) ;
#16315 = DIRECTION ( 'NONE',  ( 1.000000000000000000, 0.000000000000000000, 0.000000000000000000 ) ) ;
#16316 = ORIENTED_EDGE ( 'NONE', *, *, #8812, .F. ) ;
#16317 = EDGE_LOOP ( 'NONE', ( #9942, #6065, #2063, #10721 ) ) ;
#16318 = CARTESIAN_POINT ( 'NONE',  ( 10.00000000000000000, 15.32665449651924661, 91.22241316115426457 ) ) ;
#16319 = ORIENTED_EDGE ( 'NONE', *, *, #14156, .T. ) ;
#16320 = CARTESIAN_POINT ( 'NONE',  ( 5.000000000000000000, -81.34229909304701778, 33.57723005635337898 ) ) ;
#16321 = VECTOR ( 'NONE', #13582, 1000.000000000000000 ) ;
#16322 = FACE_OUTER_BOUND ( 'NONE', #4208, .T. ) ;
#16323 = LINE ( 'NONE', #11349, #21283 ) ;
#16324 = CARTESIAN_POINT ( 'NONE',  ( 0.000000000000000000, 56.34908017029645322, -63.71789861856395731 ) ) ;
#16325 = VECTOR ( 'NONE', #19005, 1000.000000000000000 ) ;
#16326 = AXIS2_PLACEMENT_3D ( 'NONE', #17009, #18457, #106 ) ;
#16327 = ADVANCED_FACE ( 'NONE', ( #9808 ), #5069, .F. ) ;
#16328 = DIRECTION ( 'NONE',  ( -1.000000000000000000, -0.000000000000000000, -0.000000000000000000 ) ) ;
#16329 = ADVANCED_FACE ( 'NONE', ( #4632 ), #19769, .F. ) ;
#16330 = CARTESIAN_POINT ( 'NONE',  ( 0.000000000000000000, 0.000000000000000000, 0.000000000000000000 ) ) ;
#16331 = AXIS2_PLACEMENT_3D ( 'NONE', #1479, #14955, #20053 ) ;
#16332 = CARTESIAN_POINT ( 'NONE',  ( 0.000000000000000000, -5.479102470011078196, 87.82926298292112222 ) ) ;
#16333 = CARTESIAN_POINT ( 'NONE',  ( 10.00000000000000000, 0.000000000000000000, 0.000000000000000000 ) ) ;
#16334 = ADVANCED_FACE ( 'NONE', ( #13125 ), #13235, .F. ) ;
#16335 = DIRECTION ( 'NONE',  ( 0.000000000000000000, 0.3420201433256630508, 0.9396926207859104263 ) ) ;
#16336 = ORIENTED_EDGE ( 'NONE', *, *, #20845, .T. ) ;
#16337 = AXIS2_PLACEMENT_3D ( 'NONE', #14893, #4958, #11694 ) ;
#16338 = ORIENTED_EDGE ( 'NONE', *, *, #9509, .T. ) ;
#16339 = VERTEX_POINT ( 'NONE', #18445 ) ;
#16340 = EDGE_CURVE ( 'NONE', #18743, #5507, #11102, .T. ) ;
#16341 = ORIENTED_EDGE ( 'NONE', *, *, #143, .T. ) ;
#16342 = AXIS2_PLACEMENT_3D ( 'NONE', #794, #16159, #6345 ) ;
#16343 = ORIENTED_EDGE ( 'NONE', *, *, #11895, .F. ) ;
#16344 = EDGE_CURVE ( 'NONE', #8622, #5258, #2632, .T. ) ;
#16345 = DIRECTION ( 'NONE',  ( 0.000000000000000000, 0.000000000000000000, 1.000000000000000000 ) ) ;
#16346 = ORIENTED_EDGE ( 'NONE', *, *, #10276, .F. ) ;
#16347 = LINE ( 'NONE', #2772, #12423 ) ;
#16348 = CARTESIAN_POINT ( 'NONE',  ( 10.00000000000000000, 0.000000000000000000, 100.0000000000000000 ) ) ;
#16349 = CIRCLE ( 'NONE', #13891, 12.00000000000000178 ) ;
#16350 = CARTESIAN_POINT ( 'NONE',  ( 10.00000000000000000, 0.000000000000000000, 0.000000000000000000 ) ) ;
#16351 = DIRECTION ( 'NONE',  ( 1.000000000000000000, -0.000000000000000000, -0.000000000000000000 ) ) ;
#16352 = CARTESIAN_POINT ( 'NONE',  ( 10.00000000000000000, -87.17509410653602231, -30.93441398372672069 ) ) ;
#16353 = EDGE_CURVE ( 'NONE', #18259, #15128, #20295, .T. ) ;
#16354 = CARTESIAN_POINT ( 'NONE',  ( 0.000000000000000000, -52.25832601289046409, -70.80301803122840454 ) ) ;
#16355 = DIRECTION ( 'NONE',  ( -1.000000000000000000, 0.000000000000000000, 0.000000000000000000 ) ) ;
#16356 = CIRCLE ( 'NONE', #20605, 44.99999999999998579 ) ;
#16357 = EDGE_CURVE ( 'NONE', #11720, #12094, #13581, .T. ) ;
#16358 = VERTEX_POINT ( 'NONE', #6520 ) ;
#16359 = AXIS2_PLACEMENT_3D ( 'NONE', #10773, #2268, #12330 ) ;
#16360 = DIRECTION ( 'NONE',  ( -1.000000000000000000, 0.000000000000000000, 0.000000000000000000 ) ) ;
#16361 = VERTEX_POINT ( 'NONE', #4850 ) ;
#16362 = ORIENTED_EDGE ( 'NONE', *, *, #14596, .F. ) ;
#16363 = LINE ( 'NONE', #13050, #8414 ) ;
#16364 = ADVANCED_FACE ( 'NONE', ( #10251 ), #19567, .T. ) ;
#16365 = FACE_OUTER_BOUND ( 'NONE', #17840, .T. ) ;
#16366 = VECTOR ( 'NONE', #12086, 1000.000000000000000 ) ;
#16367 = ORIENTED_EDGE ( 'NONE', *, *, #21329, .F. ) ;
#16368 = DIRECTION ( 'NONE',  ( 0.000000000000000000, -2.035408878479454078E-14, -1.000000000000000000 ) ) ;
#16369 = ORIENTED_EDGE ( 'NONE', *, *, #12879, .T. ) ;
#16370 = ADVANCED_FACE ( 'NONE', ( #13678 ), #1944, .T. ) ;
#16371 = ORIENTED_EDGE ( 'NONE', *, *, #4077, .F. ) ;
#16372 = APPLICATION_PROTOCOL_DEFINITION ( 'draft international standard', 'automotive_design', 1998, #13199 ) ;
#16373 = VECTOR ( 'NONE', #20736, 1000.000000000000000 ) ;
#16374 = CARTESIAN_POINT ( 'NONE',  ( 10.00000000000000000, -27.07404830566967746, -4.815694066514710769 ) ) ;
#16375 = VERTEX_POINT ( 'NONE', #20631 ) ;
#16376 = ORIENTED_EDGE ( 'NONE', *, *, #20414, .T. ) ;
#16377 = FACE_OUTER_BOUND ( 'NONE', #10422, .T. ) ;
#16378 = VECTOR ( 'NONE', #10311, 1000.000000000000000 ) ;
#16379 = CYLINDRICAL_SURFACE ( 'NONE', #8805, 45.00000000000000000 ) ;
#16380 = EDGE_CURVE ( 'NONE', #6192, #5341, #12513, .T. ) ;
#16381 = CYLINDRICAL_SURFACE ( 'NONE', #7595, 6.500000000000000000 ) ;
#16382 = CYLINDRICAL_SURFACE ( 'NONE', #8055, 44.99999999999998579 ) ;
#16383 =( LENGTH_UNIT ( ) NAMED_UNIT ( * ) SI_UNIT ( .MILLI., .METRE. ) );
#16384 = CARTESIAN_POINT ( 'NONE',  ( 10.00000000000000000, 27.87320266523557777, 88.20158487341770126 ) ) ;
#16385 = CARTESIAN_POINT ( 'NONE',  ( 10.00000000000000000, 23.37352460145283217, 21.85585385440887762 ) ) ;
#16386 = CARTESIAN_POINT ( 'NONE',  ( 10.49999999999999822, 1.285879139104720633E-15, 0.000000000000000000 ) ) ;
#16387 = CARTESIAN_POINT ( 'NONE',  ( 0.000000000000000000, -78.01214607583727911, -33.90124636420193838 ) ) ;
#16388 = AXIS2_PLACEMENT_3D ( 'NONE', #15347, #1874, #4672 ) ;
#16389 = EDGE_CURVE ( 'NONE', #13540, #2135, #16401, .T. ) ;
#16390 = ORIENTED_EDGE ( 'NONE', *, *, #21463, .T. ) ;
#16391 = VECTOR ( 'NONE', #5026, 1000.000000000000000 ) ;
#16392 = VERTEX_POINT ( 'NONE', #13790 ) ;
#16393 = CARTESIAN_POINT ( 'NONE',  ( 0.000000000000000000, -67.05625154133495869, 63.71729851637790176 ) ) ;
#16394 = DIRECTION ( 'NONE',  ( 1.000000000000000000, 0.000000000000000000, 0.000000000000000000 ) ) ;
#16395 = CARTESIAN_POINT ( 'NONE',  ( 10.00000000000000000, 81.97107881582226696, -22.71412948308482171 ) ) ;
#16396 = VERTEX_POINT ( 'NONE', #1970 ) ;
#16397 = SHAPE_REPRESENTATION_RELATIONSHIP ( 'NONE' , 'NONE' ,  #14169, #2505 ) ;
#16398 = AXIS2_PLACEMENT_3D ( 'NONE', #19428, #6073, #16230 ) ;
#16399 = ORIENTED_EDGE ( 'NONE', *, *, #48, .F. ) ;
#16400 = EDGE_LOOP ( 'NONE', ( #1915, #4385, #98, #586 ) ) ;
#16401 = CIRCLE ( 'NONE', #17105, 88.00000000000000000 ) ;
#16402 = ORIENTED_EDGE ( 'NONE', *, *, #1265, .T. ) ;
#16403 = CARTESIAN_POINT ( 'NONE',  ( -8.000000000000007105, 0.000000000000000000, 0.000000000000000000 ) ) ;
#16404 = FACE_OUTER_BOUND ( 'NONE', #3670, .T. ) ;
#16405 = ORIENTED_EDGE ( 'NONE', *, *, #11468, .F. ) ;
#16406 = AXIS2_PLACEMENT_3D ( 'NONE', #13218, #19970, #4836 ) ;
#16407 = EDGE_CURVE ( 'NONE', #13052, #10717, #3692, .T. ) ;
#16408 = FACE_OUTER_BOUND ( 'NONE', #6109, .T. ) ;
#16409 = DIRECTION ( 'NONE',  ( 0.000000000000000000, 0.000000000000000000, -1.000000000000000000 ) ) ;
#16410 = DIRECTION ( 'NONE',  ( 1.000000000000000000, 0.000000000000000000, 0.000000000000000000 ) ) ;
#16411 = DIRECTION ( 'NONE',  ( 0.000000000000000000, 0.000000000000000000, 1.000000000000000000 ) ) ;
#16412 = VECTOR ( 'NONE', #17667, 1000.000000000000000 ) ;
#16413 = FACE_OUTER_BOUND ( 'NONE', #10732, .T. ) ;
#16414 = DIRECTION ( 'NONE',  ( 0.000000000000000000, -0.9945218953682722907, -0.1045284632676635739 ) ) ;
#16415 = AXIS2_PLACEMENT_3D ( 'NONE', #21499, #8130, #18301 ) ;
#16416 = VERTEX_POINT ( 'NONE', #3618 ) ;
#16417 = DIRECTION ( 'NONE',  ( -1.000000000000000000, 0.000000000000000000, 0.000000000000000000 ) ) ;
#16418 = DIRECTION ( 'NONE',  ( -1.000000000000000000, 0.000000000000000000, -0.000000000000000000 ) ) ;
#16419 = VECTOR ( 'NONE', #16174, 1000.000000000000000 ) ;
#16420 = ORIENTED_EDGE ( 'NONE', *, *, #5321, .F. ) ;
#16421 = CIRCLE ( 'NONE', #1593, 45.00000000000000000 ) ;
#16422 = CIRCLE ( 'NONE', #2304, 92.50099999999999056 ) ;
#16423 = DIRECTION ( 'NONE',  ( -1.000000000000000000, 0.000000000000000000, 0.000000000000000000 ) ) ;
#16424 = AXIS2_PLACEMENT_3D ( 'NONE', #11163, #6205, #14694 ) ;
#16425 = ORIENTED_EDGE ( 'NONE', *, *, #20890, .T. ) ;
#16426 = DIRECTION ( 'NONE',  ( 0.000000000000000000, 0.9271838545667858700, 0.3746065934159160116 ) ) ;
#16427 = DIRECTION ( 'NONE',  ( 0.000000000000000000, 0.000000000000000000, 1.000000000000000000 ) ) ;
#16428 = ADVANCED_FACE ( 'NONE', ( #2083 ), #12865, .T. ) ;
#16429 = ORIENTED_EDGE ( 'NONE', *, *, #11503, .T. ) ;
#16430 = DIRECTION ( 'NONE',  ( 1.000000000000000000, 0.000000000000000000, -0.000000000000000000 ) ) ;
#16431 = ORIENTED_EDGE ( 'NONE', *, *, #20965, .F. ) ;
#16432 = ORIENTED_EDGE ( 'NONE', *, *, #15812, .T. ) ;
#16433 = CIRCLE ( 'NONE', #11481, 92.50100000000000477 ) ;
#16434 = DIRECTION ( 'NONE',  ( 0.000000000000000000, 0.000000000000000000, -1.000000000000000000 ) ) ;
#16435 = AXIS2_PLACEMENT_3D ( 'NONE', #5443, #2225, #15375 ) ;
#16436 = VERTEX_POINT ( 'NONE', #15443 ) ;
#16437 = DIRECTION ( 'NONE',  ( 1.000000000000000000, 0.000000000000000000, 0.000000000000000000 ) ) ;
#16438 = DIRECTION ( 'NONE',  ( 1.000000000000000000, 0.000000000000000000, 0.000000000000000000 ) ) ;
#16439 = DIRECTION ( 'NONE',  ( -1.000000000000000000, 0.000000000000000000, -0.000000000000000000 ) ) ;
#16440 = VECTOR ( 'NONE', #19385, 1000.000000000000000 ) ;
#16441 = DIRECTION ( 'NONE',  ( 0.000000000000000000, 0.000000000000000000, -1.000000000000000000 ) ) ;
#16442 = PRODUCT_RELATED_PRODUCT_CATEGORY ( 'part', '', ( #11974 ) ) ;
#16443 = AXIS2_PLACEMENT_3D ( 'NONE', #3693, #11985, #15399 ) ;
#16444 = AXIS2_PLACEMENT_3D ( 'NONE', #16023, #12601, #13939 ) ;
#16445 = SHAPE_REPRESENTATION ( 'radial cylindrical roller bearing_iso_ISO 15 RCR - 17200 - 54,SI,NC,54', ( #15567 ), #14522 ) ;
#16446 = DIRECTION ( 'NONE',  ( -1.000000000000000000, 0.000000000000000000, 0.000000000000000000 ) ) ;
#16447 = CARTESIAN_POINT ( 'NONE',  ( 2.799999999999996714, 60.00000000000000000, -15.00000000000000000 ) ) ;
#16448 = DIRECTION ( 'NONE',  ( 1.000000000000000000, 0.000000000000000000, 0.000000000000000000 ) ) ;
#16449 = DIRECTION ( 'NONE',  ( 1.000000000000000000, 0.000000000000000000, 0.000000000000000000 ) ) ;
#16450 = CARTESIAN_POINT ( 'NONE',  ( -10.00000000000000000, 0.000000000000000000, 0.000000000000000000 ) ) ;
#16451 = LINE ( 'NONE', #8064, #3414 ) ;
#16452 = ORIENTED_EDGE ( 'NONE', *, *, #18133, .F. ) ;
#16453 = CIRCLE ( 'NONE', #21737, 44.99999999999999289 ) ;
#16454 = ORIENTED_EDGE ( 'NONE', *, *, #15389, .T. ) ;
#16455 = CIRCLE ( 'NONE', #3068, 44.99999999999998579 ) ;
#16456 = ORIENTED_EDGE ( 'NONE', *, *, #9044, .F. ) ;
#16457 = ORIENTED_EDGE ( 'NONE', *, *, #7937, .F. ) ;
#16458 = EDGE_CURVE ( 'NONE', #14138, #797, #18528, .T. ) ;
#16459 = ORIENTED_EDGE ( 'NONE', *, *, #5969, .F. ) ;
#16460 = DIRECTION ( 'NONE',  ( 0.000000000000000000, 0.000000000000000000, -1.000000000000000000 ) ) ;
#16461 = ORIENTED_EDGE ( 'NONE', *, *, #18689, .T. ) ;
#16462 = DIRECTION ( 'NONE',  ( 0.000000000000000000, 0.000000000000000000, 1.000000000000000000 ) ) ;
#16463 = DIRECTION ( 'NONE',  ( -1.000000000000000000, -0.000000000000000000, 0.000000000000000000 ) ) ;
#16464 = EDGE_CURVE ( 'NONE', #11867, #3268, #14281, .T. ) ;
#16465 = FACE_OUTER_BOUND ( 'NONE', #10885, .T. ) ;
#16466 = AXIS2_PLACEMENT_3D ( 'NONE', #8775, #5571, #3481 ) ;
#16467 = LINE ( 'NONE', #16249, #12641 ) ;
#16468 = AXIS2_PLACEMENT_3D ( 'NONE', #5504, #20434, #2180 ) ;
#16469 = CARTESIAN_POINT ( 'NONE',  ( 10.00000000000000000, -19.85071254963791176, 20.01672328094525000 ) ) ;
#16470 = AXIS2_PLACEMENT_3D ( 'NONE', #10947, #14374, #5994 ) ;
#16471 = DIRECTION ( 'NONE',  ( -1.000000000000000000, -0.000000000000000000, 0.000000000000000000 ) ) ;
#16472 = EDGE_CURVE ( 'NONE', #9671, #18821, #4752, .T. ) ;
#16473 = DIRECTION ( 'NONE',  ( 1.000000000000000000, 0.000000000000000000, 0.000000000000000000 ) ) ;
#16474 = VERTEX_POINT ( 'NONE', #13567 ) ;
#16475 = DIRECTION ( 'NONE',  ( 0.000000000000000000, 0.000000000000000000, 1.000000000000000000 ) ) ;
#16476 = VERTEX_POINT ( 'NONE', #8594 ) ;
#16477 = ORIENTED_EDGE ( 'NONE', *, *, #7726, .F. ) ;
#16478 = CIRCLE ( 'NONE', #14002, 88.00000000000000000 ) ;
#16479 = CYLINDRICAL_SURFACE ( 'NONE', #15553, 44.99999999999999289 ) ;
#16480 = EDGE_CURVE ( 'NONE', #6845, #11540, #20322, .T. ) ;
#16481 = ORIENTED_EDGE ( 'NONE', *, *, #7726, .T. ) ;
#16482 = EDGE_CURVE ( 'NONE', #18882, #769, #15712, .T. ) ;
#16483 = VECTOR ( 'NONE', #8712, 1000.000000000000000 ) ;
#16484 = EDGE_CURVE ( 'NONE', #3028, #19897, #10467, .T. ) ;
#16485 = DIRECTION ( 'NONE',  ( 0.000000000000000000, 0.000000000000000000, -1.000000000000000000 ) ) ;
#16486 = ORIENTED_EDGE ( 'NONE', *, *, #16458, .F. ) ;
#16487 = ORIENTED_EDGE ( 'NONE', *, *, #12164, .T. ) ;
#16488 = AXIS2_PLACEMENT_3D ( 'NONE', #14675, #1087, #9802 ) ;
#16489 = CONTEXT_DEPENDENT_SHAPE_REPRESENTATION ( #5009, #1193 ) ;
#16490 = DIRECTION ( 'NONE',  ( -1.000000000000000000, -0.000000000000000000, 0.000000000000000000 ) ) ;
#16491 = EDGE_CURVE ( 'NONE', #17402, #21395, #17123, .T. ) ;
#16492 = ORIENTED_EDGE ( 'NONE', *, *, #9493, .T. ) ;
#16493 = LINE ( 'NONE', #17939, #7222 ) ;
#16494 = DIRECTION ( 'NONE',  ( 1.000000000000000000, 0.000000000000000000, 0.000000000000000000 ) ) ;
#16495 = CARTESIAN_POINT ( 'NONE',  ( 10.00000000000000000, 30.71797041605808687, 82.46457599186561538 ) ) ;
#16496 = CYLINDRICAL_SURFACE ( 'NONE', #1542, 88.00000000000000000 ) ;
#16497 = LINE ( 'NONE', #8107, #18581 ) ;
#16498 = LINE ( 'NONE', #1773, #163 ) ;
#16499 = CARTESIAN_POINT ( 'NONE',  ( 0.000000000000000000, 0.000000000000000000, -5.000000000000000000 ) ) ;
#16500 = CARTESIAN_POINT ( 'NONE',  ( 5.000000000000002665, 87.44637528609675314, -9.855528870797686025 ) ) ;
#16501 = EDGE_CURVE ( 'NONE', #6777, #4022, #13943, .T. ) ;
#16502 = DIRECTION ( 'NONE',  ( -1.000000000000000000, 0.000000000000000000, 0.000000000000000000 ) ) ;
#16503 = CIRCLE ( 'NONE', #8038, 44.99999999999999289 ) ;
#16504 = AXIS2_PLACEMENT_3D ( 'NONE', #3238, #8119, #2817 ) ;
#16505 = ORIENTED_EDGE ( 'NONE', *, *, #7093, .F. ) ;
#16506 = CIRCLE ( 'NONE', #19325, 5.633200000000004870 ) ;
#16507 = EDGE_CURVE ( 'NONE', #15910, #9924, #18889, .T. ) ;
#16508 = ORIENTED_EDGE ( 'NONE', *, *, #20433, .T. ) ;
#16509 = ADVANCED_FACE ( 'NONE', ( #5614 ), #19089, .F. ) ;
#16510 = CARTESIAN_POINT ( 'NONE',  ( 10.00000000000000000, 19.85071254963803611, -20.01672328094512565 ) ) ;
#16511 = CARTESIAN_POINT ( 'NONE',  ( 0.000000000000000000, 0.000000000000000000, 0.000000000000000000 ) ) ;
#16512 = ORIENTED_EDGE ( 'NONE', *, *, #19588, .T. ) ;
#16513 = DIRECTION ( 'NONE',  ( -1.000000000000000000, 0.000000000000000000, -0.000000000000000000 ) ) ;
#16514 = ORIENTED_EDGE ( 'NONE', *, *, #20161, .F. ) ;
#16515 = VERTEX_POINT ( 'NONE', #11914 ) ;
#16516 = EDGE_CURVE ( 'NONE', #2769, #1245, #13594, .T. ) ;
#16517 = ORIENTED_EDGE ( 'NONE', *, *, #20011, .T. ) ;
#16518 = ORIENTED_EDGE ( 'NONE', *, *, #16937, .T. ) ;
#16519 = CIRCLE ( 'NONE', #6303, 11.99999999999999822 ) ;
#16520 = CARTESIAN_POINT ( 'NONE',  ( 10.00000000000000000, -80.18694381077126820, 28.37681241246628616 ) ) ;
#16521 = DIRECTION ( 'NONE',  ( 1.000000000000000000, 0.000000000000000000, 0.000000000000000000 ) ) ;
#16522 = AXIS2_PLACEMENT_3D ( 'NONE', #10513, #17371, #8962 ) ;
#16523 = ORIENTED_EDGE ( 'NONE', *, *, #2840, .F. ) ;
#16524 = CYLINDRICAL_SURFACE ( 'NONE', #9673, 44.99999999999998579 ) ;
#16525 = FACE_OUTER_BOUND ( 'NONE', #19245, .T. ) ;
#16526 = DIRECTION ( 'NONE',  ( -1.000000000000000000, 0.000000000000000000, -0.000000000000000000 ) ) ;
#16527 = DIRECTION ( 'NONE',  ( 0.000000000000000000, 0.000000000000000000, 1.000000000000000000 ) ) ;
#16528 = FACE_OUTER_BOUND ( 'NONE', #17415, .T. ) ;
#16529 = CARTESIAN_POINT ( 'NONE',  ( 5.000000000000000000, 72.58367602204188529, 49.75550195834890843 ) ) ;
#16530 = UNCERTAINTY_MEASURE_WITH_UNIT (LENGTH_MEASURE( 1.000000000000000082E-05 ), #15634, 'distance_accuracy_value', 'NONE');
#16531 = VERTEX_POINT ( 'NONE', #2395 ) ;
#16532 = EDGE_CURVE ( 'NONE', #11363, #1889, #5717, .T. ) ;
#16533 = DIRECTION ( 'NONE',  ( 0.000000000000000000, 0.000000000000000000, 1.000000000000000000 ) ) ;
#16534 = AXIS2_PLACEMENT_3D ( 'NONE', #13359, #21431, #11370 ) ;
#16535 = DIRECTION ( 'NONE',  ( 0.000000000000000000, 0.000000000000000000, -1.000000000000000000 ) ) ;
#16536 = VECTOR ( 'NONE', #1123, 1000.000000000000000 ) ;
#16537 = ORIENTED_EDGE ( 'NONE', *, *, #7761, .F. ) ;
#16538 = EDGE_CURVE ( 'NONE', #879, #20835, #843, .T. ) ;
#16539 = AXIS2_PLACEMENT_3D ( 'NONE', #2672, #17930, #9396 ) ;
#16540 = CIRCLE ( 'NONE', #16888, 45.00000000000000000 ) ;
#16541 = EDGE_CURVE ( 'NONE', #5399, #5754, #15355, .T. ) ;
#16542 = LINE ( 'NONE', #11334, #21766 ) ;
#16543 = ORIENTED_EDGE ( 'NONE', *, *, #19998, .T. ) ;
#16544 = DIRECTION ( 'NONE',  ( 0.000000000000000000, -0.9848077530122096857, 0.1736481776669207000 ) ) ;
#16545 = DIRECTION ( 'NONE',  ( -1.000000000000000000, 0.000000000000000000, 0.000000000000000000 ) ) ;
#16546 = ORIENTED_EDGE ( 'NONE', *, *, #21344, .T. ) ;
#16547 = DIRECTION ( 'NONE',  ( 0.000000000000000000, 0.000000000000000000, 1.000000000000000000 ) ) ;
#16548 = EDGE_LOOP ( 'NONE', ( #21157, #13056, #10607, #8826 ) ) ;
#16549 = ORIENTED_EDGE ( 'NONE', *, *, #12983, .T. ) ;
#16550 = AXIS2_PLACEMENT_3D ( 'NONE', #21394, #19734, #4600 ) ;
#16551 = CARTESIAN_POINT ( 'NONE',  ( 10.00000000000000000, 2.481790431840499966, -92.46770094066590673 ) ) ;
#16552 = ORIENTED_EDGE ( 'NONE', *, *, #9479, .F. ) ;
#16553 = CARTESIAN_POINT ( 'NONE',  ( 10.00000000000000000, 21.69483248597444813, -16.89761061231758177 ) ) ;
#16554 = CIRCLE ( 'NONE', #8430, 45.00000000000000000 ) ;
#16555 = DIRECTION ( 'NONE',  ( -1.000000000000000000, 0.000000000000000000, 0.000000000000000000 ) ) ;
#16556 = DIRECTION ( 'NONE',  ( -1.000000000000000000, 0.000000000000000000, 0.000000000000000000 ) ) ;
#16557 = DIRECTION ( 'NONE',  ( -1.000000000000000000, -0.000000000000000000, -0.000000000000000000 ) ) ;
#16558 = TOROIDAL_SURFACE ( 'NONE', #21147, 101.1000000000000512, 1.100000000000009859 ) ;
#16559 = PRODUCT_DEFINITION_SHAPE ( 'NONE', 'NONE',  #381 ) ;
#16560 = DIRECTION ( 'NONE',  ( 0.000000000000000000, -0.6427876096865299260, -0.7660444431189857850 ) ) ;
#16561 = CARTESIAN_POINT ( 'NONE',  ( 10.00000000000000000, -22.77465461094663368, -15.41136296218110147 ) ) ;
#16562 = DIRECTION ( 'NONE',  ( -0.000000000000000000, -1.000000000000000000, -0.000000000000000000 ) ) ;
#16563 = CYLINDRICAL_SURFACE ( 'NONE', #12958, 92.50100000000000477 ) ;
#16564 = DIRECTION ( 'NONE',  ( 1.000000000000000000, 0.000000000000000000, 0.000000000000000000 ) ) ;
#16565 = DIRECTION ( 'NONE',  ( 1.000000000000000000, 0.000000000000000000, 0.000000000000000000 ) ) ;
#16566 = CARTESIAN_POINT ( 'NONE',  ( -1.114300000000000290, 0.000000000000000000, 0.000000000000000000 ) ) ;
#16567 = AXIS2_PLACEMENT_3D ( 'NONE', #12734, #1136, #19474 ) ;
#16568 = ORIENTED_EDGE ( 'NONE', *, *, #16793, .F. ) ;
#16569 = AXIS2_PLACEMENT_3D ( 'NONE', #12602, #892, #17485 ) ;
#16570 = ORIENTED_EDGE ( 'NONE', *, *, #8904, .F. ) ;
#16571 = VECTOR ( 'NONE', #10330, 1000.000000000000000 ) ;
#16572 = ORIENTED_EDGE ( 'NONE', *, *, #8672, .F. ) ;
#16573 = VERTEX_POINT ( 'NONE', #12881 ) ;
#16574 = EDGE_LOOP ( 'NONE', ( #1100, #7284, #20615, #2935 ) ) ;
#16575 = DIRECTION ( 'NONE',  ( -1.000000000000000000, -0.000000000000000000, 0.000000000000000000 ) ) ;
#16576 = ORIENTED_EDGE ( 'NONE', *, *, #7094, .T. ) ;
#16577 = CARTESIAN_POINT ( 'NONE',  ( 0.000000000000000000, 0.000000000000000000, 25.00000000000000000 ) ) ;
#16578 = CARTESIAN_POINT ( 'NONE',  ( 10.00000000000000000, 0.000000000000000000, 0.000000000000000000 ) ) ;
#16579 = DIRECTION ( 'NONE',  ( -1.000000000000000000, -0.000000000000000000, -0.000000000000000000 ) ) ;
#16580 = DIRECTION ( 'NONE',  ( -0.000000000000000000, -0.000000000000000000, -1.000000000000000000 ) ) ;
#16581 = DIRECTION ( 'NONE',  ( 0.000000000000000000, -2.312964634635743213E-14, -1.000000000000000000 ) ) ;
#16582 = VECTOR ( 'NONE', #16417, 1000.000000000000000 ) ;
#16583 = CARTESIAN_POINT ( 'NONE',  ( 1.139999999999998570, 8.422079734756228398E-16, 6.866799999999992465 ) ) ;
#16584 = CYLINDRICAL_SURFACE ( 'NONE', #3823, 45.00000000000000000 ) ;
#16585 = ADVANCED_FACE ( 'NONE', ( #9340 ), #14437, .T. ) ;
#16586 = ORIENTED_EDGE ( 'NONE', *, *, #16307, .T. ) ;
#16587 = LINE ( 'NONE', #4877, #2679 ) ;
#16588 = ORIENTED_EDGE ( 'NONE', *, *, #20708, .T. ) ;
#16589 = EDGE_CURVE ( 'NONE', #8158, #3795, #17542, .T. ) ;
#16590 = ORIENTED_EDGE ( 'NONE', *, *, #6724, .T. ) ;
#16591 = FACE_OUTER_BOUND ( 'NONE', #105, .T. ) ;
#16592 = VERTEX_POINT ( 'NONE', #7590 ) ;
#16593 = CIRCLE ( 'NONE', #10941, 11.99999999999999822 ) ;
#16594 = CARTESIAN_POINT ( 'NONE',  ( 0.000000000000000000, -66.01871308925505843, 64.79170103522999113 ) ) ;
#16595 = VERTEX_POINT ( 'NONE', #956 ) ;
#16596 = ORIENTED_EDGE ( 'NONE', *, *, #16994, .T. ) ;
#16597 = CONTEXT_DEPENDENT_SHAPE_REPRESENTATION ( #8694, #6511 ) ;
#16598 = CARTESIAN_POINT ( 'NONE',  ( 0.000000000000000000, -60.65655256511276860, 59.63197188857500919 ) ) ;
#16599 = ORIENTED_EDGE ( 'NONE', *, *, #7446, .F. ) ;
#16600 = CARTESIAN_POINT ( 'NONE',  ( 8.899999999999987921, 0.000000000000000000, 0.000000000000000000 ) ) ;
#16601 = LINE ( 'NONE', #8202, #6797 ) ;
#16602 = DIRECTION ( 'NONE',  ( 0.000000000000000000, 0.000000000000000000, 1.000000000000000000 ) ) ;
#16603 = DIRECTION ( 'NONE',  ( -1.000000000000000000, -0.000000000000000000, -0.000000000000000000 ) ) ;
#16604 = CARTESIAN_POINT ( 'NONE',  ( 0.000000000000000000, 0.000000000000000000, 0.000000000000000000 ) ) ;
#16605 = PLANE ( 'NONE',  #2238 ) ;
#16606 = DIRECTION ( 'NONE',  ( 0.000000000000000000, 0.6427876096865353661, 0.7660444431189813441 ) ) ;
#16607 = DIRECTION ( 'NONE',  ( 1.000000000000000000, -0.000000000000000000, -0.000000000000000000 ) ) ;
#16608 = ADVANCED_FACE ( 'NONE', ( #21068 ), #4050, .T. ) ;
#16609 = EDGE_CURVE ( 'NONE', #2662, #3420, #4381, .T. ) ;
#16610 = EDGE_CURVE ( 'NONE', #10503, #3599, #4417, .T. ) ;
#16611 = CIRCLE ( 'NONE', #7098, 11.99999999999999822 ) ;
#16612 = EDGE_LOOP ( 'NONE', ( #1932, #14776 ) ) ;
#16613 = EDGE_CURVE ( 'NONE', #10884, #715, #17488, .T. ) ;
#16614 = DIRECTION ( 'NONE',  ( 0.000000000000000000, 0.000000000000000000, 1.000000000000000000 ) ) ;
#16615 = CYLINDRICAL_SURFACE ( 'NONE', #20808, 92.50100000000000477 ) ;
#16616 = ORIENTED_EDGE ( 'NONE', *, *, #12658, .T. ) ;
#16617 = AXIS2_PLACEMENT_3D ( 'NONE', #3260, #8464, #9992 ) ;
#16618 = DIRECTION ( 'NONE',  ( -1.000000000000000000, 0.000000000000000000, 0.000000000000000000 ) ) ;
#16619 = AXIS2_PLACEMENT_3D ( 'NONE', #20893, #17694, #7757 ) ;
#16620 = VERTEX_POINT ( 'NONE', #15977 ) ;
#16621 = SURFACE_STYLE_FILL_AREA ( #16837 ) ;
#16622 = EDGE_CURVE ( 'NONE', #12772, #18178, #16421, .T. ) ;
#16623 = VERTEX_POINT ( 'NONE', #14211 ) ;
#16624 = DIRECTION ( 'NONE',  ( 0.000000000000000000, 0.000000000000000000, 1.000000000000000000 ) ) ;
#16625 = VERTEX_POINT ( 'NONE', #14327 ) ;
#16626 = ORIENTED_EDGE ( 'NONE', *, *, #4059, .T. ) ;
#16627 =( GEOMETRIC_REPRESENTATION_CONTEXT ( 3 ) GLOBAL_UNCERTAINTY_ASSIGNED_CONTEXT ( ( #20067 ) ) GLOBAL_UNIT_ASSIGNED_CONTEXT ( ( #9761, #12861, #9319 ) ) REPRESENTATION_CONTEXT ( 'NONE', 'WORKASPACE' ) );
#16628 = DIRECTION ( 'NONE',  ( 0.000000000000000000, 0.000000000000000000, -1.000000000000000000 ) ) ;
#16629 = LINE ( 'NONE', #20057, #3010 ) ;
#16630 = VERTEX_POINT ( 'NONE', #14111 ) ;
#16631 = ADVANCED_FACE ( 'NONE', ( #19633 ), #10057, .T. ) ;
#16632 = DIRECTION ( 'NONE',  ( 0.000000000000000000, 0.000000000000000000, 1.000000000000000000 ) ) ;
#16633 = CARTESIAN_POINT ( 'NONE',  ( 0.000000000000000000, -41.89587599971600440, 77.38692120905457728 ) ) ;
#16634 = DIRECTION ( 'NONE',  ( 0.000000000000000000, 0.000000000000000000, 1.000000000000000000 ) ) ;
#16635 = CARTESIAN_POINT ( 'NONE',  ( 10.00000000000000000, -81.55207211302094095, 24.17537951050038814 ) ) ;
#16636 = DIRECTION ( 'NONE',  ( -0.000000000000000000, 0.000000000000000000, -1.000000000000000000 ) ) ;
#16637 = DIRECTION ( 'NONE',  ( 1.000000000000000000, 0.000000000000000000, 0.000000000000000000 ) ) ;
#16638 = VERTEX_POINT ( 'NONE', #7807 ) ;
#16639 = CARTESIAN_POINT ( 'NONE',  ( 10.00000000000000000, -57.47876254627099257, -62.70072803846446163 ) ) ;
#16640 = EDGE_CURVE ( 'NONE', #8199, #8870, #2723, .T. ) ;
#16641 = CARTESIAN_POINT ( 'NONE',  ( 10.00000000000000000, 8.134922360107273320, -84.67002113262471141 ) ) ;
#16642 = ORIENTED_EDGE ( 'NONE', *, *, #7828, .T. ) ;
#16643 = FACE_OUTER_BOUND ( 'NONE', #1950, .T. ) ;
#16644 = ORIENTED_EDGE ( 'NONE', *, *, #8647, .F. ) ;
#16645 = DIRECTION ( 'NONE',  ( 0.8831157194574072999, 0.000000000000000000, -0.4691552259617553511 ) ) ;
#16646 = DIRECTION ( 'NONE',  ( 0.000000000000000000, 0.000000000000000000, 1.000000000000000000 ) ) ;
#16647 = ORIENTED_EDGE ( 'NONE', *, *, #2861, .F. ) ;
#16648 = EDGE_CURVE ( 'NONE', #15753, #9954, #18548, .T. ) ;
#16649 = EDGE_LOOP ( 'NONE', ( #1707, #5490, #10302, #11688 ) ) ;
#16650 = ORIENTED_EDGE ( 'NONE', *, *, #3710, .T. ) ;
#16651 = CARTESIAN_POINT ( 'NONE',  ( -90.00000000000000000, 1.284654492305574008E-14, 104.9000000000000341 ) ) ;
#16652 = EDGE_CURVE ( 'NONE', #910, #16782, #20317, .T. ) ;
#16653 = ORIENTED_EDGE ( 'NONE', *, *, #21373, .T. ) ;
#16654 = DIRECTION ( 'NONE',  ( 0.000000000000000000, 0.1391731009600591928, 0.9902680687415711391 ) ) ;
#16655 = DIRECTION ( 'NONE',  ( 1.000000000000000000, 0.000000000000000000, 0.000000000000000000 ) ) ;
#16656 = CARTESIAN_POINT ( 'NONE',  ( 10.00000000000000000, 0.000000000000000000, 0.000000000000000000 ) ) ;
#16657 = DIRECTION ( 'NONE',  ( -1.000000000000000000, -0.000000000000000000, -0.000000000000000000 ) ) ;
#16658 = EDGE_CURVE ( 'NONE', #797, #6729, #14298, .T. ) ;
#16659 = CARTESIAN_POINT ( 'NONE',  ( -1.129531546211723025, 0.000000000000000000, -5.612499999999999822 ) ) ;
#16660 = ADVANCED_FACE ( 'NONE', ( #19513 ), #7384, .F. ) ;
#16661 = DIRECTION ( 'NONE',  ( 1.000000000000000000, 0.000000000000000000, 0.000000000000000000 ) ) ;
#16662 = CARTESIAN_POINT ( 'NONE',  ( 0.000000000000000000, -75.27139873020921357, 53.76477968147791131 ) ) ;
#16663 = DIRECTION ( 'NONE',  ( 0.000000000000000000, -1.000000000000000000, 0.000000000000000000 ) ) ;
#16664 = CIRCLE ( 'NONE', #2535, 44.99999999999998579 ) ;
#16665 = EDGE_CURVE ( 'NONE', #16727, #4382, #5850, .T. ) ;
#16666 = DIRECTION ( 'NONE',  ( 0.000000000000000000, 0.000000000000000000, 1.000000000000000000 ) ) ;
#16667 = DIRECTION ( 'NONE',  ( 0.000000000000000000, -0.000000000000000000, -1.000000000000000000 ) ) ;
#16668 = VERTEX_POINT ( 'NONE', #8243 ) ;
#16669 = DIRECTION ( 'NONE',  ( -1.000000000000000000, -0.000000000000000000, 0.000000000000000000 ) ) ;
#16670 = ORIENTED_EDGE ( 'NONE', *, *, #8938, .F. ) ;
#16671 = ORIENTED_EDGE ( 'NONE', *, *, #14596, .T. ) ;
#16672 = AXIS2_PLACEMENT_3D ( 'NONE', #14937, #21679, #20031 ) ;
#16673 = ORIENTED_EDGE ( 'NONE', *, *, #10930, .F. ) ;
#16674 = ORIENTED_EDGE ( 'NONE', *, *, #56, .F. ) ;
#16675 = LINE ( 'NONE', #21648, #2411 ) ;
#16676 = ORIENTED_EDGE ( 'NONE', *, *, #6425, .T. ) ;
#16677 = DIRECTION ( 'NONE',  ( -1.000000000000000000, -0.000000000000000000, -0.000000000000000000 ) ) ;
#16678 = DIRECTION ( 'NONE',  ( -1.000000000000000000, 0.000000000000000000, -0.000000000000000000 ) ) ;
#16679 = CIRCLE ( 'NONE', #7861, 32.00000000000000000 ) ;
#16680 = DIRECTION ( 'NONE',  ( -1.000000000000000000, -0.000000000000000000, -0.000000000000000000 ) ) ;
#16681 = FACE_OUTER_BOUND ( 'NONE', #8819, .T. ) ;
#16682 = LINE ( 'NONE', #7965, #11891 ) ;
#16683 = DIRECTION ( 'NONE',  ( 0.000000000000000000, -0.6427876096865458022, 0.7660444431189725734 ) ) ;
#16684 = CIRCLE ( 'NONE', #3285, 44.99999999999998579 ) ;
#16685 = ORIENTED_EDGE ( 'NONE', *, *, #5392, .F. ) ;
#16686 = CARTESIAN_POINT ( 'NONE',  ( 10.00000000000000000, -74.74361964203200159, -40.60271866773624083 ) ) ;
#16687 = AXIS2_PLACEMENT_3D ( 'NONE', #15132, #15026, #10162 ) ;
#16688 = AXIS2_PLACEMENT_3D ( 'NONE', #15671, #5632, #19104 ) ;
#16689 = ORIENTED_EDGE ( 'NONE', *, *, #9175, .T. ) ;
#16690 = CIRCLE ( 'NONE', #20580, 45.00000000000000711 ) ;
#16691 = VERTEX_POINT ( 'NONE', #20071 ) ;
#16692 = DIRECTION ( 'NONE',  ( -1.000000000000000000, -0.000000000000000000, -0.000000000000000000 ) ) ;
#16693 = VERTEX_POINT ( 'NONE', #11331 ) ;
#16694 = DIRECTION ( 'NONE',  ( 0.000000000000000000, 0.000000000000000000, -1.000000000000000000 ) ) ;
#16695 = ORIENTED_EDGE ( 'NONE', *, *, #20011, .F. ) ;
#16696 = ORIENTED_EDGE ( 'NONE', *, *, #20149, .F. ) ;
#16697 = DIRECTION ( 'NONE',  ( 1.000000000000000000, 0.000000000000000000, -0.000000000000000000 ) ) ;
#16698 = AXIS2_PLACEMENT_3D ( 'NONE', #5061, #11798, #16560 ) ;
#16699 = EDGE_LOOP ( 'NONE', ( #19285, #4055, #9704, #14478 ) ) ;
#16700 = EDGE_CURVE ( 'NONE', #12429, #6477, #205, .T. ) ;
#16701 = CARTESIAN_POINT ( 'NONE',  ( 0.000000000000000000, -36.60317927562628881, 76.78148674856751654 ) ) ;
#16702 = CARTESIAN_POINT ( 'NONE',  ( 0.000000000000000000, 30.24235385705238244, 10.45944707835117882 ) ) ;
#16703 = AXIS2_PLACEMENT_3D ( 'NONE', #7025, #8781, #5255 ) ;
#16704 = DIRECTION ( 'NONE',  ( 0.000000000000000000, 0.000000000000000000, 1.000000000000000000 ) ) ;
#16705 = DIRECTION ( 'NONE',  ( 0.000000000000000000, 0.000000000000000000, 1.000000000000000000 ) ) ;
#16706 =( NAMED_UNIT ( * ) PLANE_ANGLE_UNIT ( ) SI_UNIT ( $, .RADIAN. ) );
#16707 = EDGE_CURVE ( 'NONE', #18401, #993, #2938, .T. ) ;
#16708 = AXIS2_PLACEMENT_3D ( 'NONE', #19469, #17822, #7773 ) ;
#16709 = CARTESIAN_POINT ( 'NONE',  ( 10.00000000000000000, -84.90234713953981327, -5.175025661884713912 ) ) ;
#16710 = DIRECTION ( 'NONE',  ( 0.000000000000000000, 0.6946583704589984753, -0.7193398003386500816 ) ) ;
#16711 = CYLINDRICAL_SURFACE ( 'NONE', #5942, 92.50100000000000477 ) ;
#16712 = EDGE_LOOP ( 'NONE', ( #10170, #17352, #5276, #18288 ) ) ;
#16713 = AXIS2_PLACEMENT_3D ( 'NONE', #16635, #13426, #4698 ) ;
#16714 = FACE_OUTER_BOUND ( 'NONE', #12539, .T. ) ;
#16715 = APPLICATION_CONTEXT ( 'automotive_design' ) ;
#16716 = AXIS2_PLACEMENT_3D ( 'NONE', #11529, #14838, #11305 ) ;
#16717 = CARTESIAN_POINT ( 'NONE',  ( 0.000000000000000000, 0.000000000000000000, 0.000000000000000000 ) ) ;
#16718 = EDGE_LOOP ( 'NONE', ( #10589, #2971 ) ) ;
#16719 = CARTESIAN_POINT ( 'NONE',  ( 0.000000000000000000, 67.05625154133539922, -63.71729851637743280 ) ) ;
#16720 = VERTEX_POINT ( 'NONE', #21515 ) ;
#16721 = CIRCLE ( 'NONE', #9644, 44.99999999999998579 ) ;
#16722 =( LENGTH_UNIT ( ) NAMED_UNIT ( * ) SI_UNIT ( .MILLI., .METRE. ) );
#16723 = ORIENTED_EDGE ( 'NONE', *, *, #2716, .T. ) ;
#16724 = CARTESIAN_POINT ( 'NONE',  ( 0.000000000000000000, 12.46320060045724354, 29.47318494484032669 ) ) ;
#16725 = ORIENTED_EDGE ( 'NONE', *, *, #8200, .T. ) ;
#16726 = EDGE_CURVE ( 'NONE', #1655, #1066, #11830, .T. ) ;
#16727 = VERTEX_POINT ( 'NONE', #8032 ) ;
#16728 = CARTESIAN_POINT ( 'NONE',  ( -1.114300000000000068, 0.000000000000000000, 0.000000000000000000 ) ) ;
#16729 = DIRECTION ( 'NONE',  ( -1.000000000000000000, -0.000000000000000000, -0.000000000000000000 ) ) ;
#16730 = ORIENTED_EDGE ( 'NONE', *, *, #8306, .F. ) ;
#16731 = CARTESIAN_POINT ( 'NONE',  ( -10.00000000000000000, 0.000000000000000000, 0.000000000000000000 ) ) ;
#16732 = CARTESIAN_POINT ( 'NONE',  ( 0.000000000000000000, 56.34908017029559346, 63.71789861856471049 ) ) ;
#16733 = CARTESIAN_POINT ( 'NONE',  ( 10.00000000000000000, -68.93609746931124960, -54.69748134696530428 ) ) ;
#16734 = DIRECTION ( 'NONE',  ( -1.000000000000000000, -0.000000000000000000, 0.000000000000000000 ) ) ;
#16735 = DIRECTION ( 'NONE',  ( -1.000000000000000000, 0.000000000000000000, -0.000000000000000000 ) ) ;
#16736 = CARTESIAN_POINT ( 'NONE',  ( 0.000000000000000000, 10.41137886060106865, 91.91321010181850681 ) ) ;
#16737 = ORIENTED_EDGE ( 'NONE', *, *, #3767, .T. ) ;
#16738 = CIRCLE ( 'NONE', #3335, 88.00000000000000000 ) ;
#16739 = DIRECTION ( 'NONE',  ( 0.000000000000000000, 0.8987940462991680368, -0.4383711467890751279 ) ) ;
#16740 = EDGE_CURVE ( 'NONE', #16266, #289, #2644, .T. ) ;
#16741 = CARTESIAN_POINT ( 'NONE',  ( 10.00000000000000000, 68.36541360927260769, -50.60987712331631627 ) ) ;
#16742 = VERTEX_POINT ( 'NONE', #2836 ) ;
#16743 = EDGE_CURVE ( 'NONE', #12032, #15273, #3706, .T. ) ;
#16744 = CARTESIAN_POINT ( 'NONE',  ( 5.000000000000000000, -24.17932380791732427, 20.96092317126997884 ) ) ;
#16745 = ORIENTED_EDGE ( 'NONE', *, *, #18671, .F. ) ;
#16746 = CIRCLE ( 'NONE', #5808, 6.728125000000022560 ) ;
#16747 = DIRECTION ( 'NONE',  ( 1.000000000000000000, 0.000000000000000000, 0.000000000000000000 ) ) ;
#16748 = AXIS2_PLACEMENT_3D ( 'NONE', #9168, #20678, #2329 ) ;
#16749 = CARTESIAN_POINT ( 'NONE',  ( 0.000000000000000000, 7.240962358591573889, 31.16999300804317130 ) ) ;
#16750 = ORIENTED_EDGE ( 'NONE', *, *, #4906, .T. ) ;
#16751 = CIRCLE ( 'NONE', #7234, 32.00000000000000000 ) ;
#16752 = CARTESIAN_POINT ( 'NONE',  ( 0.000000000000000000, 27.87320266523671819, -88.20158487341731757 ) ) ;
#16753 = AXIS2_PLACEMENT_3D ( 'NONE', #1822, #1716, #8558 ) ;
#16755 = ADVANCED_FACE ( 'NONE', ( #9663 ), #8144, .F. ) ;
#16754 = ORIENTED_EDGE ( 'NONE', *, *, #21484, .T. ) ;
#16756 = ORIENTED_EDGE ( 'NONE', *, *, #7676, .T. ) ;
#16757 = EDGE_CURVE ( 'NONE', #14363, #16630, #5134, .T. ) ;
#16758 = EDGE_LOOP ( 'NONE', ( #2406, #14860, #15390, #8971 ) ) ;
#16759 = EDGE_CURVE ( 'NONE', #10503, #5372, #9698, .T. ) ;
#16760 = CARTESIAN_POINT ( 'NONE',  ( -5.000000000000000000, 5.000000000000000000, 9.999999999999998224 ) ) ;
#16761 = AXIS2_PLACEMENT_3D ( 'NONE', #9147, #19529, #7497 ) ;
#16762 = ORIENTED_EDGE ( 'NONE', *, *, #15930, .T. ) ;
#16763 = CARTESIAN_POINT ( 'NONE',  ( 5.000000000000000000, -47.19205848891713373, -74.27590198428171675 ) ) ;
#16764 = EDGE_CURVE ( 'NONE', #12792, #7793, #17137, .T. ) ;
#16765 = DIRECTION ( 'NONE',  ( -1.000000000000000000, 0.000000000000000000, -0.000000000000000000 ) ) ;
#16766 = FACE_OUTER_BOUND ( 'NONE', #4533, .T. ) ;
#16767 = FACE_OUTER_BOUND ( 'NONE', #13379, .T. ) ;
#16768 = DIRECTION ( 'NONE',  ( 1.000000000000000000, 0.000000000000000000, 0.000000000000000000 ) ) ;
#16769 = AXIS2_PLACEMENT_3D ( 'NONE', #2503, #11231, #17985 ) ;
#16770 = DIRECTION ( 'NONE',  ( -0.000000000000000000, -0.000000000000000000, 1.000000000000000000 ) ) ;
#16771 = VECTOR ( 'NONE', #15385, 1000.000000000000000 ) ;
#16772 = AXIS2_PLACEMENT_3D ( 'NONE', #9224, #19506, #2715 ) ;
#16773 = CARTESIAN_POINT ( 'NONE',  ( 10.00000000000000000, 0.000000000000000000, 0.000000000000000000 ) ) ;
#16774 = EDGE_CURVE ( 'NONE', #447, #17747, #16049, .T. ) ;
#16775 = CIRCLE ( 'NONE', #17127, 92.50100000000000477 ) ;
#16776 = DIRECTION ( 'NONE',  ( -1.000000000000000000, -0.000000000000000000, 0.000000000000000000 ) ) ;
#16777 = ADVANCED_FACE ( 'NONE', ( #4824 ), #6603, .F. ) ;
#16778 = ADVANCED_FACE ( 'NONE', ( #12995 ), #3267, .F. ) ;
#16779 = CARTESIAN_POINT ( 'NONE',  ( 0.000000000000000000, 5.479102470011647519, -87.82926298292107958 ) ) ;
#16780 = ORIENTED_EDGE ( 'NONE', *, *, #5042, .F. ) ;
#16781 = FILL_AREA_STYLE_COLOUR ( '', #14433 ) ;
#16782 = VERTEX_POINT ( 'NONE', #14770 ) ;
#16783 = VECTOR ( 'NONE', #16961, 1000.000000000000000 ) ;
#16784 = DIRECTION ( 'NONE',  ( 0.000000000000000000, 0.000000000000000000, -1.000000000000000000 ) ) ;
#16785 = EDGE_CURVE ( 'NONE', #8011, #9734, #14320, .T. ) ;
#16786 = VERTEX_POINT ( 'NONE', #6718 ) ;
#16787 = VERTEX_POINT ( 'NONE', #1174 ) ;
#16788 = VECTOR ( 'NONE', #7242, 1000.000000000000000 ) ;
#16789 = AXIS2_PLACEMENT_3D ( 'NONE', #17294, #2144, #8877 ) ;
#16790 = VERTEX_POINT ( 'NONE', #4496 ) ;
#16791 = AXIS2_PLACEMENT_3D ( 'NONE', #17554, #17664, #15893 ) ;
#16792 = DIRECTION ( 'NONE',  ( 0.000000000000000000, -1.079383496163346864E-14, -1.000000000000000000 ) ) ;
#16793 = EDGE_CURVE ( 'NONE', #8475, #8452, #11504, .T. ) ;
#16794 = ORIENTED_EDGE ( 'NONE', *, *, #15651, .F. ) ;
#16795 = DIRECTION ( 'NONE',  ( 0.000000000000000000, 0.06975647374411846069, 0.9975640502598246417 ) ) ;
#16796 = LINE ( 'NONE', #107, #9971 ) ;
#16797 = ADVANCED_FACE ( 'NONE', ( #3055 ), #10733, .F. ) ;
#16798 = CARTESIAN_POINT ( 'NONE',  ( 10.00000000000000000, 1.959304526717801975, 27.42911093658675981 ) ) ;
#16799 =( NAMED_UNIT ( * ) SI_UNIT ( $, .STERADIAN. ) SOLID_ANGLE_UNIT ( ) );
#16800 = DIRECTION ( 'NONE',  ( 1.000000000000000000, 0.000000000000000000, 0.000000000000000000 ) ) ;
#16801 = DIRECTION ( 'NONE',  ( 0.000000000000000000, 0.000000000000000000, -1.000000000000000000 ) ) ;
#16802 = AXIS2_PLACEMENT_3D ( 'NONE', #21425, #7832, #4411 ) ;
#16803 = ORIENTED_EDGE ( 'NONE', *, *, #8959, .T. ) ;
#16804 = EDGE_CURVE ( 'NONE', #13666, #10884, #1978, .T. ) ;
#16805 = AXIS2_PLACEMENT_3D ( 'NONE', #6355, #9525, #16273 ) ;
#16806 = DIRECTION ( 'NONE',  ( 0.000000000000000000, 0.000000000000000000, 1.000000000000000000 ) ) ;
#16807 = CIRCLE ( 'NONE', #14642, 44.99999999999999289 ) ;
#16808 = VERTEX_POINT ( 'NONE', #20177 ) ;
#16809 = EDGE_CURVE ( 'NONE', #14602, #20731, #691, .T. ) ;
#16810 = ORIENTED_EDGE ( 'NONE', *, *, #18011, .T. ) ;
#16811 = CARTESIAN_POINT ( 'NONE',  ( 10.00000000000000000, -4.294029059350045863, 27.86182539015965176 ) ) ;
#16812 = ORIENTED_EDGE ( 'NONE', *, *, #18830, .F. ) ;
#16813 = DIRECTION ( 'NONE',  ( -1.000000000000000000, 0.000000000000000000, 0.000000000000000000 ) ) ;
#16814 = ORIENTED_EDGE ( 'NONE', *, *, #12162, .F. ) ;
#16815 = VERTEX_POINT ( 'NONE', #14155 ) ;
#16816 = CONTEXT_DEPENDENT_SHAPE_REPRESENTATION ( #5725, #1554 ) ;
#16817 = DIRECTION ( 'NONE',  ( -1.000000000000000000, -0.000000000000000000, -0.000000000000000000 ) ) ;
#16818 = ORIENTED_EDGE ( 'NONE', *, *, #9760, .F. ) ;
#16819 = AXIS2_PLACEMENT_3D ( 'NONE', #20323, #1320, #4738 ) ;
#16820 = AXIS2_PLACEMENT_3D ( 'NONE', #9385, #7753, #17589 ) ;
#16821 = CYLINDRICAL_SURFACE ( 'NONE', #781, 12.00000000000000000 ) ;
#16822 = DIRECTION ( 'NONE',  ( 0.000000000000000000, -0.2756373558169870064, -0.9612616959383222248 ) ) ;
#16823 = CARTESIAN_POINT ( 'NONE',  ( 10.00000000000000000, -52.34334029047928993, 76.26670130689468863 ) ) ;
#16824 = CYLINDRICAL_SURFACE ( 'NONE', #15373, 11.99999999999999822 ) ;
#16825 = CARTESIAN_POINT ( 'NONE',  ( 0.000000000000000000, -82.02147376274642454, -42.76579056660944644 ) ) ;
#16826 = FACE_OUTER_BOUND ( 'NONE', #18767, .T. ) ;
#16827 = CARTESIAN_POINT ( 'NONE',  ( 0.000000000000000000, -43.18649929580243452, 73.28107340219401067 ) ) ;
#16828 = EDGE_LOOP ( 'NONE', ( #19695, #6176, #17936, #7774 ) ) ;
#16829 = EDGE_CURVE ( 'NONE', #21336, #8720, #9013, .T. ) ;
#16830 = AXIS2_PLACEMENT_3D ( 'NONE', #13813, #17017, #345 ) ;
#16831 = CIRCLE ( 'NONE', #11537, 5.000000000000000000 ) ;
#16832 = DIRECTION ( 'NONE',  ( 0.000000000000000000, 0.8660254037844398178, -0.4999999999999980016 ) ) ;
#16833 = CARTESIAN_POINT ( 'NONE',  ( 5.000000000000000000, 83.89484365856912973, 26.56417150042976161 ) ) ;
#16834 = ORIENTED_EDGE ( 'NONE', *, *, #2017, .F. ) ;
#16835 = CARTESIAN_POINT ( 'NONE',  ( 5.000000000000000000, -78.80192417387900150, -39.16958956249377621 ) ) ;
#16836 = ORIENTED_EDGE ( 'NONE', *, *, #6760, .T. ) ;
#16837 = FILL_AREA_STYLE ('',( #17056 ) ) ;
#16838 = ORIENTED_EDGE ( 'NONE', *, *, #12054, .F. ) ;
#16839 = DIRECTION ( 'NONE',  ( 0.000000000000000000, 0.000000000000000000, 1.000000000000000000 ) ) ;
#16840 = VERTEX_POINT ( 'NONE', #13762 ) ;
#16841 = ORIENTED_EDGE ( 'NONE', *, *, #12151, .F. ) ;
#16842 = DIRECTION ( 'NONE',  ( -1.000000000000000000, 0.000000000000000000, -0.000000000000000000 ) ) ;
#16843 = CARTESIAN_POINT ( 'NONE',  ( 10.00000000000000000, -3.786343810537759147, 27.23708136986050832 ) ) ;
#16844 = ORIENTED_EDGE ( 'NONE', *, *, #581, .T. ) ;
#16845 = AXIS2_PLACEMENT_3D ( 'NONE', #9574, #9477, #21419 ) ;
#16846 = DIRECTION ( 'NONE',  ( 1.000000000000000000, -0.000000000000000000, -0.000000000000000000 ) ) ;
#16847 = CARTESIAN_POINT ( 'NONE',  ( 10.00000000000000000, 39.87723064937119233, 83.46401306393586594 ) ) ;
#16848 = AXIS2_PLACEMENT_3D ( 'NONE', #19489, #11094, #4472 ) ;
#16849 = DIRECTION ( 'NONE',  ( 0.000000000000000000, 0.000000000000000000, -1.000000000000000000 ) ) ;
#16850 = DIRECTION ( 'NONE',  ( -1.000000000000000000, -0.000000000000000000, -0.000000000000000000 ) ) ;
#16851 = AXIS2_PLACEMENT_3D ( 'NONE', #14516, #7887, #12519 ) ;
#16852 = DIRECTION ( 'NONE',  ( 1.000000000000000000, 0.000000000000000000, 0.000000000000000000 ) ) ;
#16853 = LINE ( 'NONE', #6597, #3208 ) ;
#16854 = ORIENTED_EDGE ( 'NONE', *, *, #5813, .F. ) ;
#16855 = DIRECTION ( 'NONE',  ( 0.000000000000000000, 0.000000000000000000, 1.000000000000000000 ) ) ;
#16856 = DIRECTION ( 'NONE',  ( 0.000000000000000000, 0.000000000000000000, -1.000000000000000000 ) ) ;
#16857 = ADVANCED_FACE ( 'NONE', ( #9179 ), #5037, .T. ) ;
#16858 = ORIENTED_EDGE ( 'NONE', *, *, #4354, .F. ) ;
#16859 = PRODUCT_DEFINITION_CONTEXT ( 'detailed design', #19692, 'design' ) ;
#16860 = ORIENTED_EDGE ( 'NONE', *, *, #2482, .T. ) ;
#16861 = AXIS2_PLACEMENT_3D ( 'NONE', #3332, #13275, #11840 ) ;
#16862 = CARTESIAN_POINT ( 'NONE',  ( 0.000000000000000000, -21.98203405400942856, -17.64965094506566246 ) ) ;
#16863 = VECTOR ( 'NONE', #1584, 1000.000000000000000 ) ;
#16864 = CIRCLE ( 'NONE', #4167, 92.50100000000000477 ) ;
#16865 = FACE_OUTER_BOUND ( 'NONE', #9945, .T. ) ;
#16866 = AXIS2_PLACEMENT_3D ( 'NONE', #5003, #9964, #141 ) ;
#16867 = ORIENTED_EDGE ( 'NONE', *, *, #2550, .F. ) ;
#16868 = EDGE_CURVE ( 'NONE', #5777, #16638, #4090, .T. ) ;
#16869 = CARTESIAN_POINT ( 'NONE',  ( 150.0000507999999968, 4.000000000000000000, 1.000000000000000000 ) ) ;
#16870 = ORIENTED_EDGE ( 'NONE', *, *, #19732, .F. ) ;
#16871 = ORIENTED_EDGE ( 'NONE', *, *, #13503, .T. ) ;
#16872 = ORIENTED_EDGE ( 'NONE', *, *, #7577, .F. ) ;
#16873 = PLANE ( 'NONE',  #4360 ) ;
#16874 = VERTEX_POINT ( 'NONE', #65 ) ;
#16875 = VECTOR ( 'NONE', #10293, 1000.000000000000000 ) ;
#16876 = EDGE_CURVE ( 'NONE', #4200, #5362, #13649, .T. ) ;
#16877 = DIRECTION ( 'NONE',  ( 1.000000000000000000, 0.000000000000000000, 0.000000000000000000 ) ) ;
#16878 = LINE ( 'NONE', #18862, #13556 ) ;
#16879 = CARTESIAN_POINT ( 'NONE',  ( -8.000000000000007105, 0.000000000000000000, 0.000000000000000000 ) ) ;
#16880 = CARTESIAN_POINT ( 'NONE',  ( 0.000000000000000000, -14.02138820414853448, -83.89630571862299746 ) ) ;
#16881 = FACE_OUTER_BOUND ( 'NONE', #672, .T. ) ;
#16882 = CIRCLE ( 'NONE', #15105, 44.99999999999999289 ) ;
#16883 = AXIS2_PLACEMENT_3D ( 'NONE', #2231, #15929, #10847 ) ;
#16884 = CARTESIAN_POINT ( 'NONE',  ( 0.000000000000000000, 0.000000000000000000, 0.000000000000000000 ) ) ;
#16885 = DIRECTION ( 'NONE',  ( 0.000000000000000000, 0.000000000000000000, 1.000000000000000000 ) ) ;
#16886 = VECTOR ( 'NONE', #21037, 1000.000000000000000 ) ;
#16887 = AXIS2_PLACEMENT_3D ( 'NONE', #18374, #3217, #16694 ) ;
#16888 = AXIS2_PLACEMENT_3D ( 'NONE', #9275, #16025, #893 ) ;
#16889 = CARTESIAN_POINT ( 'NONE',  ( 10.00000000000000000, 0.000000000000000000, 0.000000000000000000 ) ) ;
#16890 = ADVANCED_FACE ( 'NONE', ( #11775 ), #5773, .T. ) ;
#16891 = CARTESIAN_POINT ( 'NONE',  ( -1.200000000000006617, 0.000000000000000000, 0.000000000000000000 ) ) ;
#16892 = EDGE_CURVE ( 'NONE', #16010, #1387, #18218, .T. ) ;
#16893 = ADVANCED_FACE ( 'NONE', ( #20289 ), #3377, .T. ) ;
#16894 = DIRECTION ( 'NONE',  ( -1.000000000000000000, -0.000000000000000000, -0.000000000000000000 ) ) ;
#16895 = ORIENTED_EDGE ( 'NONE', *, *, #12715, .F. ) ;
#16896 = EDGE_CURVE ( 'NONE', #20213, #7466, #21025, .T. ) ;
#16897 = FACE_OUTER_BOUND ( 'NONE', #21589, .T. ) ;
#16898 = ORIENTED_EDGE ( 'NONE', *, *, #19492, .F. ) ;
#16899 = DIRECTION ( 'NONE',  ( -1.000000000000000000, 0.000000000000000000, 0.000000000000000000 ) ) ;
#16900 = ORIENTED_EDGE ( 'NONE', *, *, #16464, .T. ) ;
#16901 = CIRCLE ( 'NONE', #21487, 44.99999999999998579 ) ;
#16902 = ORIENTED_EDGE ( 'NONE', *, *, #13836, .T. ) ;
#16903 = CIRCLE ( 'NONE', #8083, 92.50100000000000477 ) ;
#16904 = AXIS2_PLACEMENT_3D ( 'NONE', #4057, #17546, #2401 ) ;
#16905 = AXIS2_PLACEMENT_3D ( 'NONE', #18228, #13232, #12910 ) ;
#16906 = ORIENTED_EDGE ( 'NONE', *, *, #11551, .T. ) ;
#16907 = EDGE_CURVE ( 'NONE', #20616, #2596, #10111, .T. ) ;
#16908 = CYLINDRICAL_SURFACE ( 'NONE', #20426, 44.99999999999998579 ) ;
#16909 = ORIENTED_EDGE ( 'NONE', *, *, #20622, .T. ) ;
#16910 = LINE ( 'NONE', #1868, #12082 ) ;
#16911 = DIRECTION ( 'NONE',  ( 0.000000000000000000, 0.7431448254773953543, -0.6691306063588570163 ) ) ;
#16912 = EDGE_CURVE ( 'NONE', #9256, #5435, #7620, .T. ) ;
#16913 = DIRECTION ( 'NONE',  ( 0.000000000000000000, 0.7431448254773953543, -0.6691306063588567943 ) ) ;
#16914 = CARTESIAN_POINT ( 'NONE',  ( 10.00000000000000000, 0.000000000000000000, 0.000000000000000000 ) ) ;
#16915 = DIRECTION ( 'NONE',  ( 0.000000000000000000, 0.5299192642331999048, 0.8480480961564290654 ) ) ;
#16916 = DIRECTION ( 'NONE',  ( 0.000000000000000000, 0.4067366430758011520, -0.9135454576426005335 ) ) ;
#16917 = DIRECTION ( 'NONE',  ( -1.000000000000000000, 0.000000000000000000, -0.000000000000000000 ) ) ;
#16918 = AXIS2_PLACEMENT_3D ( 'NONE', #5055, #16437, #8372 ) ;
#16919 = AXIS2_PLACEMENT_3D ( 'NONE', #18744, #17197, #20611 ) ;
#16920 = CIRCLE ( 'NONE', #8102, 44.99999999999999289 ) ;
#16921 = ORIENTED_EDGE ( 'NONE', *, *, #12168, .T. ) ;
#16922 = CIRCLE ( 'NONE', #3512, 45.00000000000000000 ) ;
#16923 = DIRECTION ( 'NONE',  ( 0.000000000000000000, 0.000000000000000000, -1.000000000000000000 ) ) ;
#16924 = EDGE_CURVE ( 'NONE', #11424, #2463, #19608, .T. ) ;
#16925 = ORIENTED_EDGE ( 'NONE', *, *, #2190, .T. ) ;
#16926 = EDGE_LOOP ( 'NONE', ( #18762, #4769, #18829, #6311 ) ) ;
#16927 = DIRECTION ( 'NONE',  ( 0.000000000000000000, 0.000000000000000000, -1.000000000000000000 ) ) ;
#16928 = VERTEX_POINT ( 'NONE', #18740 ) ;
#16929 = DIRECTION ( 'NONE',  ( -1.000000000000000000, 0.000000000000000000, 0.000000000000000000 ) ) ;
#16930 = ORIENTED_EDGE ( 'NONE', *, *, #6404, .F. ) ;
#16931 = VERTEX_POINT ( 'NONE', #5364 ) ;
#16932 = CIRCLE ( 'NONE', #10569, 44.99999999999999289 ) ;
#16933 = ADVANCED_FACE ( 'NONE', ( #1936 ), #18633, .T. ) ;
#16934 = DIRECTION ( 'NONE',  ( 0.000000000000000000, 0.000000000000000000, 1.000000000000000000 ) ) ;
#16935 = ORIENTED_EDGE ( 'NONE', *, *, #17211, .F. ) ;
#16936 = VECTOR ( 'NONE', #10201, 1000.000000000000000 ) ;
#16937 = EDGE_CURVE ( 'NONE', #20292, #18743, #285, .T. ) ;
#16938 = VECTOR ( 'NONE', #9131, 1000.000000000000000 ) ;
#16939 = CARTESIAN_POINT ( 'NONE',  ( 0.000000000000000000, 0.000000000000000000, 0.000000000000000000 ) ) ;
#16940 = CARTESIAN_POINT ( 'NONE',  ( 10.00000000000000000, 0.000000000000000000, 0.000000000000000000 ) ) ;
#16941 = DIRECTION ( 'NONE',  ( 0.000000000000000000, 0.000000000000000000, -1.000000000000000000 ) ) ;
#16942 = FACE_OUTER_BOUND ( 'NONE', #14097, .T. ) ;
#16943 = EDGE_CURVE ( 'NONE', #21704, #12864, #3997, .T. ) ;
#16944 = EDGE_CURVE ( 'NONE', #1536, #13081, #18565, .T. ) ;
#16945 = CARTESIAN_POINT ( 'NONE',  ( 10.00000000000000000, 0.000000000000000000, 0.000000000000000000 ) ) ;
#16946 = DIRECTION ( 'NONE',  ( 0.000000000000000000, 0.000000000000000000, 1.000000000000000000 ) ) ;
#16947 = CARTESIAN_POINT ( 'NONE',  ( 0.000000000000000000, 81.55207211302045778, 24.17537951050201883 ) ) ;
#16948 = ORIENTED_EDGE ( 'NONE', *, *, #1108, .T. ) ;
#16949 = VECTOR ( 'NONE', #21563, 1000.000000000000000 ) ;
#16950 = DIRECTION ( 'NONE',  ( 0.000000000000000000, 0.000000000000000000, 1.000000000000000000 ) ) ;
#16951 = CARTESIAN_POINT ( 'NONE',  ( 0.000000000000000000, 78.01214607583752070, 33.90124636420136994 ) ) ;
#16952 = VERTEX_POINT ( 'NONE', #19458 ) ;
#16953 = DIRECTION ( 'NONE',  ( 1.000000000000000000, 0.000000000000000000, 0.000000000000000000 ) ) ;
#16954 = ORIENTED_EDGE ( 'NONE', *, *, #17292, .T. ) ;
#16955 = PRESENTATION_STYLE_ASSIGNMENT (( #10209 ) ) ;
#16956 = ORIENTED_EDGE ( 'NONE', *, *, #19995, .F. ) ;
#16957 = CARTESIAN_POINT ( 'NONE',  ( 10.00000000000000000, 56.34908017029559346, 63.71789861856471049 ) ) ;
#16958 = ORIENTED_EDGE ( 'NONE', *, *, #276, .F. ) ;
#16959 = ORIENTED_EDGE ( 'NONE', *, *, #19896, .T. ) ;
#16960 = CARTESIAN_POINT ( 'NONE',  ( 10.00000000000000000, 41.87002153499211232, -74.04114219178001122 ) ) ;
#16961 = DIRECTION ( 'NONE',  ( 1.000000000000000000, -0.000000000000000000, -0.000000000000000000 ) ) ;
#16962 = ORIENTED_EDGE ( 'NONE', *, *, #2818, .F. ) ;
#16963 = CYLINDRICAL_SURFACE ( 'NONE', #5105, 32.00000000000000000 ) ;
#16964 = DIRECTION ( 'NONE',  ( 0.000000000000000000, 0.000000000000000000, -1.000000000000000000 ) ) ;
#16965 = DIRECTION ( 'NONE',  ( 0.000000000000000000, 0.000000000000000000, -1.000000000000000000 ) ) ;
#16966 = LINE ( 'NONE', #1927, #8610 ) ;
#16967 = LINE ( 'NONE', #6918, #2227 ) ;
#16968 = DIRECTION ( 'NONE',  ( 0.000000000000000000, 0.000000000000000000, 1.000000000000000000 ) ) ;
#16969 = ORIENTED_EDGE ( 'NONE', *, *, #19424, .F. ) ;
#16970 = FACE_OUTER_BOUND ( 'NONE', #8504, .T. ) ;
#16971 = DIRECTION ( 'NONE',  ( -1.000000000000000000, 0.000000000000000000, 0.000000000000000000 ) ) ;
#16972 = ORIENTED_EDGE ( 'NONE', *, *, #20431, .T. ) ;
#16973 = FACE_OUTER_BOUND ( 'NONE', #14935, .T. ) ;
#16974 = ORIENTED_EDGE ( 'NONE', *, *, #837, .T. ) ;
#16975 = FACE_OUTER_BOUND ( 'NONE', #16926, .T. ) ;
#16976 = AXIS2_PLACEMENT_3D ( 'NONE', #18645, #3500, #12102 ) ;
#16977 = CARTESIAN_POINT ( 'NONE',  ( 0.000000000000000000, 0.6021240089805670603, -31.99433460282943997 ) ) ;
#16978 = ORIENTED_EDGE ( 'NONE', *, *, #11677, .T. ) ;
#16979 = CARTESIAN_POINT ( 'NONE',  ( 0.000000000000000000, -81.32027326007839463, -44.08455690949136851 ) ) ;
#16980 = ORIENTED_EDGE ( 'NONE', *, *, #4077, .T. ) ;
#16981 = ORIENTED_EDGE ( 'NONE', *, *, #19982, .T. ) ;
#16982 = VERTEX_POINT ( 'NONE', #5886 ) ;
#16983 = DIRECTION ( 'NONE',  ( -1.000000000000000000, -0.000000000000000000, -0.000000000000000000 ) ) ;
#16984 = ORIENTED_EDGE ( 'NONE', *, *, #14355, .F. ) ;
#16985 = CARTESIAN_POINT ( 'NONE',  ( 10.00000000000000000, 36.39558101400249512, -80.12091913260344711 ) ) ;
#16986 = DIRECTION ( 'NONE',  ( 0.000000000000000000, 0.000000000000000000, 1.000000000000000000 ) ) ;
#16987 = CYLINDRICAL_SURFACE ( 'NONE', #11215, 104.9000000000000341 ) ;
#16988 = EDGE_CURVE ( 'NONE', #2130, #20275, #895, .T. ) ;
#16989 = CARTESIAN_POINT ( 'NONE',  ( -1.114300000000000068, 0.000000000000000000, 0.000000000000000000 ) ) ;
#16990 = CARTESIAN_POINT ( 'NONE',  ( 10.00000000000000000, -6.797690662954623875, -87.73705831432221203 ) ) ;
#16991 = CARTESIAN_POINT ( 'NONE',  ( 10.00000000000000000, 0.000000000000000000, 0.000000000000000000 ) ) ;
#16992 = CYLINDRICAL_SURFACE ( 'NONE', #5046, 11.99999999999999822 ) ;
#16993 =( GEOMETRIC_REPRESENTATION_CONTEXT ( 3 ) GLOBAL_UNCERTAINTY_ASSIGNED_CONTEXT ( ( #10483 ) ) GLOBAL_UNIT_ASSIGNED_CONTEXT ( ( #9517, #7871, #6228 ) ) REPRESENTATION_CONTEXT ( 'NONE', 'WORKASPACE' ) );
#16994 = EDGE_CURVE ( 'NONE', #4150, #8155, #11286, .T. ) ;
#16995 = DIRECTION ( 'NONE',  ( 0.000000000000000000, 0.000000000000000000, 1.000000000000000000 ) ) ;
#16996 = DIRECTION ( 'NONE',  ( 0.000000000000000000, 0.000000000000000000, 1.000000000000000000 ) ) ;
#16997 = DIRECTION ( 'NONE',  ( 0.000000000000000000, 0.000000000000000000, 1.000000000000000000 ) ) ;
#16998 = ORIENTED_EDGE ( 'NONE', *, *, #1796, .T. ) ;
#16999 = PRESENTATION_STYLE_ASSIGNMENT (( #13571 ) ) ;
#17000 = ORIENTED_EDGE ( 'NONE', *, *, #13888, .T. ) ;
#17001 = LINE ( 'NONE', #16261, #16536 ) ;
#17002 = VERTEX_POINT ( 'NONE', #11056 ) ;
#17003 = ORIENTED_EDGE ( 'NONE', *, *, #8777, .T. ) ;
#17004 = CIRCLE ( 'NONE', #765, 88.00000000000000000 ) ;
#17005 = CYLINDRICAL_SURFACE ( 'NONE', #16819, 6.887500000000022382 ) ;
#17006 = ORIENTED_EDGE ( 'NONE', *, *, #21794, .T. ) ;
#17007 = DIRECTION ( 'NONE',  ( 0.000000000000000000, -0.9271838545667908660, 0.3746065934159032440 ) ) ;
#17008 = ORIENTED_EDGE ( 'NONE', *, *, #20850, .T. ) ;
#17009 = CARTESIAN_POINT ( 'NONE',  ( 10.00000000000000000, 56.34908017029645322, -63.71789861856395731 ) ) ;
#17010 = EDGE_CURVE ( 'NONE', #13187, #4811, #1613, .T. ) ;
#17011 = EDGE_CURVE ( 'NONE', #20811, #13006, #9717, .T. ) ;
#17012 = CARTESIAN_POINT ( 'NONE',  ( 10.00000000000000000, -28.15804365424196121, -1.358152127006266197 ) ) ;
#17013 = VECTOR ( 'NONE', #11692, 1000.000000000000000 ) ;
#17014 = CARTESIAN_POINT ( 'NONE',  ( 0.000000000000000000, 0.000000000000000000, 0.000000000000000000 ) ) ;
#17015 = DIRECTION ( 'NONE',  ( -1.000000000000000000, -0.000000000000000000, 0.000000000000000000 ) ) ;
#17016 = DIRECTION ( 'NONE',  ( 1.000000000000000000, -0.000000000000000000, -0.000000000000000000 ) ) ;
#17017 = DIRECTION ( 'NONE',  ( 1.000000000000000000, 0.000000000000000000, 0.000000000000000000 ) ) ;
#17018 = DIRECTION ( 'NONE',  ( 0.000000000000000000, -0.06975647374411138302, -0.9975640502598251969 ) ) ;
#17019 = VERTEX_POINT ( 'NONE', #19792 ) ;
#17020 = DIRECTION ( 'NONE',  ( 1.000000000000000000, 0.000000000000000000, 0.000000000000000000 ) ) ;
#17021 = EDGE_CURVE ( 'NONE', #19331, #13000, #10781, .T. ) ;
#17022 = AXIS2_PLACEMENT_3D ( 'NONE', #12058, #13722, #19125 ) ;
#17023 = ORIENTED_EDGE ( 'NONE', *, *, #7327, .F. ) ;
#17024 = ORIENTED_EDGE ( 'NONE', *, *, #20558, .F. ) ;
#17025 = EDGE_CURVE ( 'NONE', #3881, #15140, #15016, .T. ) ;
#17026 = LINE ( 'NONE', #5325, #17328 ) ;
#17027 = VECTOR ( 'NONE', #11817, 1000.000000000000000 ) ;
#17028 = ORIENTED_EDGE ( 'NONE', *, *, #4046, .F. ) ;
#17029 = ORIENTED_EDGE ( 'NONE', *, *, #3840, .F. ) ;
#17030 = VERTEX_POINT ( 'NONE', #4222 ) ;
#17031 = AXIS2_PLACEMENT_3D ( 'NONE', #7827, #4192, #14676 ) ;
#17032 = DIRECTION ( 'NONE',  ( 0.000000000000000000, 0.000000000000000000, -1.000000000000000000 ) ) ;
#17033 = EDGE_CURVE ( 'NONE', #13577, #9520, #14703, .T. ) ;
#17034 = ORIENTED_EDGE ( 'NONE', *, *, #19100, .T. ) ;
#17035 = ADVANCED_FACE ( 'NONE', ( #21446 ), #10952, .F. ) ;
#17036 = DIRECTION ( 'NONE',  ( 0.000000000000000000, -0.7431448254773861395, -0.6691306063588672304 ) ) ;
#17037 = EDGE_CURVE ( 'NONE', #2668, #9323, #10074, .T. ) ;
#17038 = VECTOR ( 'NONE', #1660, 1000.000000000000000 ) ;
#17039 = CARTESIAN_POINT ( 'NONE',  ( 10.00000000000000000, 70.37753541435941429, 60.02863908169658202 ) ) ;
#17040 = CARTESIAN_POINT ( 'NONE',  ( 10.00000000000000000, 0.000000000000000000, 0.000000000000000000 ) ) ;
#17041 = CARTESIAN_POINT ( 'NONE',  ( 10.00000000000000000, -15.25521607131222268, 23.70650506194164464 ) ) ;
#17042 = LINE ( 'NONE', #11965, #19185 ) ;
#17043 = DIRECTION ( 'NONE',  ( -1.000000000000000000, 0.000000000000000000, 0.000000000000000000 ) ) ;
#17044 = FACE_OUTER_BOUND ( 'NONE', #2822, .T. ) ;
#17045 = AXIS2_PLACEMENT_3D ( 'NONE', #20222, #1663, #10 ) ;
#17046 = ORIENTED_EDGE ( 'NONE', *, *, #19145, .T. ) ;
#17047 = EDGE_CURVE ( 'NONE', #11398, #8996, #16066, .T. ) ;
#17048 = ADVANCED_FACE ( 'NONE', ( #12819 ), #9603, .T. ) ;
#17049 = CARTESIAN_POINT ( 'NONE',  ( 0.000000000000000000, 1.224646799147353217E-14, -100.0000000000000000 ) ) ;
#17050 = DIRECTION ( 'NONE',  ( -1.000000000000000000, 0.000000000000000000, 0.000000000000000000 ) ) ;
#17051 = AXIS2_PLACEMENT_3D ( 'NONE', #1518, #10134, #6512 ) ;
#17052 = VERTEX_POINT ( 'NONE', #2666 ) ;
#17053 = DIRECTION ( 'NONE',  ( 1.000000000000000000, 0.000000000000000000, 0.000000000000000000 ) ) ;
#17054 = VERTEX_POINT ( 'NONE', #17700 ) ;
#17055 = EDGE_CURVE ( 'NONE', #15636, #2214, #6570, .T. ) ;
#17056 = FILL_AREA_STYLE_COLOUR ( '', #4999 ) ;
#17057 = ORIENTED_EDGE ( 'NONE', *, *, #5006, .F. ) ;
#17058 = AXIS2_PLACEMENT_3D ( 'NONE', #6384, #11023, #16636 ) ;
#17059 = CYLINDRICAL_SURFACE ( 'NONE', #12800, 27.49900000000000233 ) ;
#17060 = VERTEX_POINT ( 'NONE', #19564 ) ;
#17061 = ORIENTED_EDGE ( 'NONE', *, *, #16726, .T. ) ;
#17062 = CYLINDRICAL_SURFACE ( 'NONE', #13574, 44.99999999999999289 ) ;
#17063 = DIRECTION ( 'NONE',  ( 0.000000000000000000, 0.000000000000000000, 1.000000000000000000 ) ) ;
#17064 = AXIS2_PLACEMENT_3D ( 'NONE', #20417, #16983, #15312 ) ;
#17065 = ADVANCED_FACE ( 'NONE', ( #18140 ), #4439, .F. ) ;
#17066 = DIRECTION ( 'NONE',  ( 1.000000000000000000, 0.000000000000000000, 0.000000000000000000 ) ) ;
#17067 = DIRECTION ( 'NONE',  ( 0.000000000000000000, 0.000000000000000000, 1.000000000000000000 ) ) ;
#17068 = DIRECTION ( 'NONE',  ( 0.000000000000000000, -0.9702957262759938084, -0.2419218955996777498 ) ) ;
#17069 = LINE ( 'NONE', #11986, #16366 ) ;
#17070 = LINE ( 'NONE', #3696, #2583 ) ;
#17071 = DIRECTION ( 'NONE',  ( -1.000000000000000000, 0.000000000000000000, 0.000000000000000000 ) ) ;
#17072 = CIRCLE ( 'NONE', #6501, 32.00000000000000000 ) ;
#17073 = ORIENTED_EDGE ( 'NONE', *, *, #8090, .F. ) ;
#17074 = CARTESIAN_POINT ( 'NONE',  ( 5.000000000000000888, 7.240962358591984227, -31.16999300804307538 ) ) ;
#17075 = AXIS2_PLACEMENT_3D ( 'NONE', #21154, #2249, #6025 ) ;
#17076 = CARTESIAN_POINT ( 'NONE',  ( 150.0000507999999968, 4.000000000000000000, -1.000000000000000000 ) ) ;
#17077 = VERTEX_POINT ( 'NONE', #7857 ) ;
#17078 = AXIS2_PLACEMENT_3D ( 'NONE', #19076, #10663, #9003 ) ;
#17079 = DIRECTION ( 'NONE',  ( -1.000000000000000000, 0.000000000000000000, -0.000000000000000000 ) ) ;
#17080 = EDGE_LOOP ( 'NONE', ( #19438, #15009, #12004, #2062, #16432, #7166 ) ) ;
#17081 = SURFACE_STYLE_FILL_AREA ( #20080 ) ;
#17082 = LINE ( 'NONE', #10654, #13726 ) ;
#17083 = ORIENTED_EDGE ( 'NONE', *, *, #17055, .T. ) ;
#17084 = ADVANCED_FACE ( 'NONE', ( #14595 ), #12717, .F. ) ;
#17085 = DIRECTION ( 'NONE',  ( 1.000000000000000000, 0.000000000000000000, 0.000000000000000000 ) ) ;
#17086 = AXIS2_PLACEMENT_3D ( 'NONE', #18946, #20280, #11876 ) ;
#17087 = ORIENTED_EDGE ( 'NONE', *, *, #16027, .F. ) ;
#17088 = ORIENTED_EDGE ( 'NONE', *, *, #6366, .F. ) ;
#17089 = ORIENTED_EDGE ( 'NONE', *, *, #20149, .T. ) ;
#17090 = CARTESIAN_POINT ( 'NONE',  ( 1.500000000000000000, 5.100000000000000533, 0.000000000000000000 ) ) ;
#17091 = ORIENTED_EDGE ( 'NONE', *, *, #18787, .T. ) ;
#17092 = DIRECTION ( 'NONE',  ( -1.000000000000000000, -0.000000000000000000, -0.000000000000000000 ) ) ;
#17093 = DIRECTION ( 'NONE',  ( 1.000000000000000000, 0.000000000000000000, 0.000000000000000000 ) ) ;
#17094 = DIRECTION ( 'NONE',  ( 0.000000000000000000, -0.9510565162951565288, 0.3090169943749382919 ) ) ;
#17095 = DIRECTION ( 'NONE',  ( 0.000000000000000000, 0.000000000000000000, 1.000000000000000000 ) ) ;
#17096 = PRODUCT_DEFINITION_SHAPE ( 'NONE', 'NONE',  #19678 ) ;
#17097 = LINE ( 'NONE', #3610, #2948 ) ;
#17098 = VECTOR ( 'NONE', #18941, 1000.000000000000000 ) ;
#17099 = LINE ( 'NONE', #5287, #11525 ) ;
#17100 = CARTESIAN_POINT ( 'NONE',  ( 10.00000000000000000, 1.959304526717801975, 27.42911093658675981 ) ) ;
#17101 = DIRECTION ( 'NONE',  ( 0.000000000000000000, 0.9945218953682737340, -0.1045284632676503622 ) ) ;
#17102 = VERTEX_POINT ( 'NONE', #8189 ) ;
#17103 = DIRECTION ( 'NONE',  ( -1.000000000000000000, -0.000000000000000000, -0.000000000000000000 ) ) ;
#17104 = DIRECTION ( 'NONE',  ( 1.000000000000000000, 0.000000000000000000, 0.000000000000000000 ) ) ;
#17105 = AXIS2_PLACEMENT_3D ( 'NONE', #8711, #3945, #12019 ) ;
#17106 = EDGE_CURVE ( 'NONE', #20086, #7542, #8088, .T. ) ;
#17107 = DIRECTION ( 'NONE',  ( -1.000000000000000000, 0.000000000000000000, 0.000000000000000000 ) ) ;
#17108 = CIRCLE ( 'NONE', #4409, 11.99999999999999822 ) ;
#17109 = EDGE_LOOP ( 'NONE', ( #21483, #18143 ) ) ;
#17110 = DIRECTION ( 'NONE',  ( 0.000000000000000000, 0.000000000000000000, 1.000000000000000000 ) ) ;
#17111 = VERTEX_POINT ( 'NONE', #6763 ) ;
#17112 = CARTESIAN_POINT ( 'NONE',  ( 0.000000000000000000, 0.000000000000000000, 0.000000000000000000 ) ) ;
#17113 = VECTOR ( 'NONE', #17773, 1000.000000000000000 ) ;
#17114 = EDGE_LOOP ( 'NONE', ( #21591, #12869, #10202, #18122 ) ) ;
#17115 = ORIENTED_EDGE ( 'NONE', *, *, #15435, .F. ) ;
#17116 = PRODUCT_RELATED_PRODUCT_CATEGORY ( 'part', '', ( #18865 ) ) ;
#17117 = EDGE_LOOP ( 'NONE', ( #3647, #14991, #16588, #1627 ) ) ;
#17118 = DIRECTION ( 'NONE',  ( -1.000000000000000000, -0.000000000000000000, -0.000000000000000000 ) ) ;
#17119 = CIRCLE ( 'NONE', #18180, 44.99999999999998579 ) ;
#17120 = ORIENTED_EDGE ( 'NONE', *, *, #3013, .F. ) ;
#17121 = DIRECTION ( 'NONE',  ( -1.000000000000000000, -0.000000000000000000, 0.000000000000000000 ) ) ;
#17122 = CARTESIAN_POINT ( 'NONE',  ( 5.000000000000000000, -47.19205848891816402, 74.27590198428104884 ) ) ;
#17123 = CIRCLE ( 'NONE', #12883, 12.00000000000000000 ) ;
#17124 = CARTESIAN_POINT ( 'NONE',  ( -8.000000000000007105, 0.000000000000000000, -113.8250000000000028 ) ) ;
#17125 = VECTOR ( 'NONE', #7909, 1000.000000000000000 ) ;
#17126 = PRODUCT_DEFINITION_CONTEXT ( 'detailed design', #774, 'design' ) ;
#17127 = AXIS2_PLACEMENT_3D ( 'NONE', #6122, #6568, #16822 ) ;
#17128 = DIRECTION ( 'NONE',  ( -1.000000000000000000, 0.000000000000000000, -0.000000000000000000 ) ) ;
#17129 = LINE ( 'NONE', #12143, #2366 ) ;
#17130 = DIRECTION ( 'NONE',  ( 1.000000000000000000, 0.000000000000000000, 0.000000000000000000 ) ) ;
#17131 = DIRECTION ( 'NONE',  ( 0.000000000000000000, 0.2079116908177599532, -0.9781476007338055778 ) ) ;
#17132 = DIRECTION ( 'NONE',  ( -1.000000000000000000, 0.000000000000000000, 0.000000000000000000 ) ) ;
#17133 = ORIENTED_EDGE ( 'NONE', *, *, #4791, .T. ) ;
#17134 = CARTESIAN_POINT ( 'NONE',  ( 0.000000000000000000, 23.37352460145313771, -21.85585385440855788 ) ) ;
#17135 = EDGE_CURVE ( 'NONE', #17002, #14785, #16, .T. ) ;
#17136 = CIRCLE ( 'NONE', #203, 44.99999999999999289 ) ;
#17137 = CIRCLE ( 'NONE', #18201, 12.00000000000000000 ) ;
#17138 = ORIENTED_EDGE ( 'NONE', *, *, #21401, .T. ) ;
#17139 = VECTOR ( 'NONE', #8654, 1000.000000000000000 ) ;
#17140 = AXIS2_PLACEMENT_3D ( 'NONE', #1490, #8234, #18411 ) ;
#17141 = VERTEX_POINT ( 'NONE', #13264 ) ;
#17142 = AXIS2_PLACEMENT_3D ( 'NONE', #15486, #7424, #14147 ) ;
#17143 = CARTESIAN_POINT ( 'NONE',  ( 0.000000000000000000, 87.17509410653667601, -30.93441398372498341 ) ) ;
#17144 = ORIENTED_EDGE ( 'NONE', *, *, #8792, .T. ) ;
#17145 = ORIENTED_EDGE ( 'NONE', *, *, #11677, .F. ) ;
#17146 = ADVANCED_FACE ( 'NONE', ( #10055 ), #14820, .T. ) ;
#17147 = DIRECTION ( 'NONE',  ( -1.000000000000000000, -0.000000000000000000, 0.000000000000000000 ) ) ;
#17148 = ORIENTED_EDGE ( 'NONE', *, *, #1230, .F. ) ;
#17149 = CYLINDRICAL_SURFACE ( 'NONE', #6452, 92.50100000000000477 ) ;
#17150 = ADVANCED_FACE ( 'NONE', ( #6867 ), #9838, .F. ) ;
#17151 = LINE ( 'NONE', #4895, #8308 ) ;
#17152 = DIRECTION ( 'NONE',  ( 0.000000000000000000, 0.000000000000000000, 1.000000000000000000 ) ) ;
#17153 = AXIS2_PLACEMENT_3D ( 'NONE', #2342, #10325, #15925 ) ;
#17154 = LINE ( 'NONE', #2013, #18936 ) ;
#17155 = CIRCLE ( 'NONE', #14321, 45.00000000000000711 ) ;
#17156 = CIRCLE ( 'NONE', #18921, 45.00000000000000000 ) ;
#17157 = LINE ( 'NONE', #8751, #16072 ) ;
#17158 = CYLINDRICAL_SURFACE ( 'NONE', #10565, 100.0000000000000284 ) ;
#17160 = AXIS2_PLACEMENT_3D ( 'NONE', #2297, #2408, #10691 ) ;
#17159 = CARTESIAN_POINT ( 'NONE',  ( 10.00000000000000000, 0.000000000000000000, 0.000000000000000000 ) ) ;
#17161 = ORIENTED_EDGE ( 'NONE', *, *, #16357, .T. ) ;
#17162 = ADVANCED_FACE ( 'NONE', ( #20127 ), #8516, .F. ) ;
#17163 = EDGE_CURVE ( 'NONE', #17734, #11955, #10458, .T. ) ;
#17164 = EDGE_CURVE ( 'NONE', #21218, #11543, #1290, .T. ) ;
#17165 = CARTESIAN_POINT ( 'NONE',  ( 10.00000000000000000, 90.63195040374188238, 18.50093422002450083 ) ) ;
#17166 = EDGE_CURVE ( 'NONE', #9664, #9397, #16453, .T. ) ;
#17167 = DIRECTION ( 'NONE',  ( -1.000000000000000000, 0.000000000000000000, 0.000000000000000000 ) ) ;
#17168 = ORIENTED_EDGE ( 'NONE', *, *, #3928, .T. ) ;
#17169 = DIRECTION ( 'NONE',  ( 0.000000000000000000, 0.000000000000000000, 1.000000000000000000 ) ) ;
#17170 = VERTEX_POINT ( 'NONE', #6549 ) ;
#17171 = SURFACE_STYLE_USAGE ( .BOTH. , #10416 ) ;
#17172 = AXIS2_PLACEMENT_3D ( 'NONE', #3099, #9828, #5495 ) ;
#17173 = CARTESIAN_POINT ( 'NONE',  ( 10.00000000000000000, 89.12061559554365431, -24.77803214283454736 ) ) ;
#17174 = ORIENTED_EDGE ( 'NONE', *, *, #18509, .T. ) ;
#17175 = ORIENTED_EDGE ( 'NONE', *, *, #4229, .T. ) ;
#17176 = DIRECTION ( 'NONE',  ( 0.000000000000000000, 0.000000000000000000, 1.000000000000000000 ) ) ;
#17177 = CARTESIAN_POINT ( 'NONE',  ( 10.00000000000000000, 86.77540292929722909, -14.62974526292624944 ) ) ;
#17178 = EDGE_CURVE ( 'NONE', #18403, #9309, #11861, .T. ) ;
#17179 = CARTESIAN_POINT ( 'NONE',  ( -10.00000000000000000, 0.000000000000000000, 0.000000000000000000 ) ) ;
#17180 = CARTESIAN_POINT ( 'NONE',  ( 0.000000000000000000, 27.26034713664097353, -7.182859710736244629 ) ) ;
#17181 = LINE ( 'NONE', #10429, #18568 ) ;
#17182 = CARTESIAN_POINT ( 'NONE',  ( 10.00000000000000000, -15.32665449651862843, -91.22241316115434984 ) ) ;
#17183 = CARTESIAN_POINT ( 'NONE',  ( 10.00000000000000000, 0.000000000000000000, 0.000000000000000000 ) ) ;
#17184 = EDGE_CURVE ( 'NONE', #13006, #6332, #14683, .T. ) ;
#17185 = CARTESIAN_POINT ( 'NONE',  ( 10.00000000000000000, 84.90234713953992696, -5.175025661882965089 ) ) ;
#17186 = AXIS2_PLACEMENT_3D ( 'NONE', #14151, #19242, #10839 ) ;
#17187 = AXIS2_PLACEMENT_3D ( 'NONE', #20062, #4930, #11664 ) ;
#17188 = AXIS2_PLACEMENT_3D ( 'NONE', #9579, #2757, #16335 ) ;
#17189 = ORIENTED_EDGE ( 'NONE', *, *, #16255, .F. ) ;
#17190 = AXIS2_PLACEMENT_3D ( 'NONE', #17895, #16446, #4402 ) ;
#17191 = CYLINDRICAL_SURFACE ( 'NONE', #1272, 44.99999999999998579 ) ;
#17192 = ORIENTED_EDGE ( 'NONE', *, *, #19018, .F. ) ;
#17193 = CARTESIAN_POINT ( 'NONE',  ( 0.000000000000000000, 86.77540292929701593, 14.62974526292747868 ) ) ;
#17194 = ORIENTED_EDGE ( 'NONE', *, *, #10385, .T. ) ;
#17195 = EDGE_CURVE ( 'NONE', #12538, #10938, #16587, .T. ) ;
#17196 = DIRECTION ( 'NONE',  ( 0.000000000000000000, -0.8987940462991619306, -0.4383711467890878399 ) ) ;
#17197 = DIRECTION ( 'NONE',  ( -1.000000000000000000, 0.000000000000000000, 0.000000000000000000 ) ) ;
#17198 = ORIENTED_EDGE ( 'NONE', *, *, #8864, .F. ) ;
#17199 = VECTOR ( 'NONE', #14351, 1000.000000000000000 ) ;
#17200 = ORIENTED_EDGE ( 'NONE', *, *, #16079, .T. ) ;
#17201 = ORIENTED_EDGE ( 'NONE', *, *, #10388, .T. ) ;
#17202 = ORIENTED_EDGE ( 'NONE', *, *, #20721, .T. ) ;
#17203 = DIRECTION ( 'NONE',  ( 0.000000000000000000, 0.000000000000000000, 1.000000000000000000 ) ) ;
#17204 = VECTOR ( 'NONE', #4462, 1000.000000000000000 ) ;
#17205 = ORIENTED_EDGE ( 'NONE', *, *, #10788, .F. ) ;
#17206 = CARTESIAN_POINT ( 'NONE',  ( 0.000000000000000000, -3.728035544475628793, -84.97818067823773447 ) ) ;
#17207 = EDGE_CURVE ( 'NONE', #13321, #2883, #14337, .T. ) ;
#17208 = DIRECTION ( 'NONE',  ( 0.000000000000000000, 0.000000000000000000, 1.000000000000000000 ) ) ;
#17209 = DIRECTION ( 'NONE',  ( -1.000000000000000000, -0.000000000000000000, -0.000000000000000000 ) ) ;
#17210 = DIRECTION ( 'NONE',  ( 0.000000000000000000, -0.9271838545667908660, 0.3746065934159032440 ) ) ;
#17211 = EDGE_CURVE ( 'NONE', #12634, #17141, #15742, .T. ) ;
#17212 = CARTESIAN_POINT ( 'NONE',  ( 10.00000000000000000, 27.82509854686811224, 4.525913221811229903 ) ) ;
#17213 = DIRECTION ( 'NONE',  ( 0.000000000000000000, 0.000000000000000000, -1.000000000000000000 ) ) ;
#17214 = DIRECTION ( 'NONE',  ( 1.000000000000000000, 0.000000000000000000, 0.000000000000000000 ) ) ;
#17215 = EDGE_CURVE ( 'NONE', #1305, #4587, #12566, .T. ) ;
#17216 = ORIENTED_EDGE ( 'NONE', *, *, #207, .F. ) ;
#17217 = EDGE_CURVE ( 'NONE', #6557, #17273, #9735, .T. ) ;
#17218 = DIRECTION ( 'NONE',  ( 0.000000000000000000, 0.000000000000000000, 1.000000000000000000 ) ) ;
#17219 = CIRCLE ( 'NONE', #18637, 27.49900000000000233 ) ;
#17220 = CARTESIAN_POINT ( 'NONE',  ( 0.000000000000000000, 1.592605004252791279, 28.14575649959894932 ) ) ;
#17221 = AXIS2_PLACEMENT_3D ( 'NONE', #6932, #2154, #5366 ) ;
#17222 = CIRCLE ( 'NONE', #981, 92.50100000000000477 ) ;
#17223 = CIRCLE ( 'NONE', #12269, 44.99999999999998579 ) ;
#17224 = DIRECTION ( 'NONE',  ( 1.000000000000000000, 0.000000000000000000, 0.000000000000000000 ) ) ;
#17225 = ORIENTED_EDGE ( 'NONE', *, *, #5961, .T. ) ;
#17226 = FACE_OUTER_BOUND ( 'NONE', #2217, .T. ) ;
#17227 = VERTEX_POINT ( 'NONE', #20350 ) ;
#17228 = DIRECTION ( 'NONE',  ( -1.000000000000000000, 0.000000000000000000, 0.000000000000000000 ) ) ;
#17229 = ORIENTED_EDGE ( 'NONE', *, *, #8506, .T. ) ;
#17230 = ORIENTED_EDGE ( 'NONE', *, *, #973, .F. ) ;
#17231 = VERTEX_POINT ( 'NONE', #11507 ) ;
#17232 = FACE_OUTER_BOUND ( 'NONE', #21267, .T. ) ;
#17233 = CIRCLE ( 'NONE', #2054, 120.0000000000000568 ) ;
#17234 = AXIS2_PLACEMENT_3D ( 'NONE', #20818, #2685, #9408 ) ;
#17235 = CARTESIAN_POINT ( 'NONE',  ( 10.00000000000000000, 84.79630770241084292, -6.691460262315676033 ) ) ;
#17236 = DIRECTION ( 'NONE',  ( 1.000000000000000000, -0.000000000000000000, -0.000000000000000000 ) ) ;
#17237 = VECTOR ( 'NONE', #15831, 1000.000000000000000 ) ;
#17238 = CIRCLE ( 'NONE', #17253, 114.9007999999999896 ) ;
#17239 = DIRECTION ( 'NONE',  ( 0.000000000000000000, -0.5299192642331944647, -0.8480480961564325071 ) ) ;
#17240 = DIRECTION ( 'NONE',  ( 0.000000000000000000, 0.000000000000000000, 1.000000000000000000 ) ) ;
#17241 = DIRECTION ( 'NONE',  ( 0.000000000000000000, 0.000000000000000000, 1.000000000000000000 ) ) ;
#17242 = CYLINDRICAL_SURFACE ( 'NONE', #19923, 92.50100000000000477 ) ;
#17243 = DIRECTION ( 'NONE',  ( 0.000000000000000000, 0.000000000000000000, 1.000000000000000000 ) ) ;
#17244 = CARTESIAN_POINT ( 'NONE',  ( 10.00000000000000000, 0.000000000000000000, 0.000000000000000000 ) ) ;
#17245 = VERTEX_POINT ( 'NONE', #15036 ) ;
#17246 = CARTESIAN_POINT ( 'NONE',  ( 0.000000000000000000, -91.70173545986527586, 12.13370160540012499 ) ) ;
#17247 = AXIS2_PLACEMENT_3D ( 'NONE', #8722, #2189, #10693 ) ;
#17248 = ORIENTED_EDGE ( 'NONE', *, *, #6678, .T. ) ;
#17249 = CIRCLE ( 'NONE', #16183, 27.49900000000000588 ) ;
#17250 = ORIENTED_EDGE ( 'NONE', *, *, #5, .T. ) ;
#17251 = AXIS2_PLACEMENT_3D ( 'NONE', #5892, #17707, #12615 ) ;
#17252 = AXIS2_PLACEMENT_3D ( 'NONE', #18948, #2044, #20396 ) ;
#17253 = AXIS2_PLACEMENT_3D ( 'NONE', #21330, #21443, #15030 ) ;
#17254 = ORIENTED_EDGE ( 'NONE', *, *, #21763, .F. ) ;
#17255 = CARTESIAN_POINT ( 'NONE',  ( 5.000000000000002665, -18.94217447942501309, -85.93715160505971085 ) ) ;
#17256 = ORIENTED_EDGE ( 'NONE', *, *, #19730, .F. ) ;
#17257 = ORIENTED_EDGE ( 'NONE', *, *, #1537, .F. ) ;
#17258 = CARTESIAN_POINT ( 'NONE',  ( 0.000000000000000000, 60.00000000000000000, 9.999999999999998224 ) ) ;
#17259 = ORIENTED_EDGE ( 'NONE', *, *, #18911, .T. ) ;
#17260 = AXIS2_PLACEMENT_3D ( 'NONE', #4492, #16298, #1170 ) ;
#17261 = CARTESIAN_POINT ( 'NONE',  ( 0.000000000000000000, -11.59241532900687233, 87.23311244498734141 ) ) ;
#17262 = CARTESIAN_POINT ( 'NONE',  ( 10.00000000000000000, 0.000000000000000000, 0.000000000000000000 ) ) ;
#17263 = CIRCLE ( 'NONE', #2426, 44.99999999999999289 ) ;
#17264 = CYLINDRICAL_SURFACE ( 'NONE', #546, 11.99999999999999822 ) ;
#17265 = CARTESIAN_POINT ( 'NONE',  ( 10.00000000000000000, -87.58454185039434492, -8.540961822682595184 ) ) ;
#17266 = EDGE_CURVE ( 'NONE', #7559, #5754, #15384, .T. ) ;
#17267 = AXIS2_PLACEMENT_3D ( 'NONE', #11453, #5163, #21835 ) ;
#17268 = DIRECTION ( 'NONE',  ( 1.000000000000000000, 0.000000000000000000, 0.000000000000000000 ) ) ;
#17269 = CIRCLE ( 'NONE', #14073, 27.49900000000000233 ) ;
#17270 = DIRECTION ( 'NONE',  ( 0.000000000000000000, 1.224646799147322392E-16, 1.000000000000000000 ) ) ;
#17271 = CARTESIAN_POINT ( 'NONE',  ( -1.500000000000000000, 15.00000000000000000, 7.000000000000000000 ) ) ;
#17272 = FACE_OUTER_BOUND ( 'NONE', #1861, .T. ) ;
#17273 = VERTEX_POINT ( 'NONE', #10278 ) ;
#17274 = EDGE_CURVE ( 'NONE', #16592, #8708, #13260, .T. ) ;
#17275 = CARTESIAN_POINT ( 'NONE',  ( 10.00000000000000000, -9.992993448021772807, 26.36019881529882980 ) ) ;
#17276 = AXIS2_PLACEMENT_3D ( 'NONE', #17206, #2068, #8804 ) ;
#17277 = DIRECTION ( 'NONE',  ( -1.000000000000000000, 0.000000000000000000, -0.000000000000000000 ) ) ;
#17278 = ORIENTED_EDGE ( 'NONE', *, *, #21533, .F. ) ;
#17279 = CIRCLE ( 'NONE', #10203, 9.999999999999998224 ) ;
#17280 = STYLED_ITEM ( 'NONE', ( #11096 ), #20833 ) ;
#17281 = CARTESIAN_POINT ( 'NONE',  ( 0.000000000000000000, 0.000000000000000000, 0.000000000000000000 ) ) ;
#17282 = AXIS2_PLACEMENT_3D ( 'NONE', #16889, #1751, #1968 ) ;
#17283 = ORIENTED_EDGE ( 'NONE', *, *, #18097, .F. ) ;
#17284 = SURFACE_SIDE_STYLE ('',( #13955 ) ) ;
#17285 = CARTESIAN_POINT ( 'NONE',  ( 10.00000000000000000, 78.83848282823907994, 48.38314403117527718 ) ) ;
#17286 = VERTEX_POINT ( 'NONE', #17134 ) ;
#17287 = ORIENTED_EDGE ( 'NONE', *, *, #12233, .T. ) ;
#17288 = CARTESIAN_POINT ( 'NONE',  ( -1.500000000000000000, 5.000000000000000000, 0.000000000000000000 ) ) ;
#17289 = DIRECTION ( 'NONE',  ( -1.000000000000000000, -0.000000000000000000, -0.000000000000000000 ) ) ;
#17290 = CARTESIAN_POINT ( 'NONE',  ( 150.0000507999999968, 2.828427124746190291, 1.000000000000000000 ) ) ;
#17291 = DIRECTION ( 'NONE',  ( -1.000000000000000000, 0.000000000000000000, 0.000000000000000000 ) ) ;
#17292 = EDGE_CURVE ( 'NONE', #20559, #13983, #231, .T. ) ;
#17293 = EDGE_CURVE ( 'NONE', #1439, #9851, #5322, .T. ) ;
#17294 = CARTESIAN_POINT ( 'NONE',  ( 0.000000000000000000, -48.19312842678424857, -70.09002648625245513 ) ) ;
#17295 = ADVANCED_FACE ( 'NONE', ( #557 ), #12258, .T. ) ;
#17296 = FACE_OUTER_BOUND ( 'NONE', #10406, .T. ) ;
#17297 = CARTESIAN_POINT ( 'NONE',  ( 5.000000000000000000, 60.65279801375431390, -63.75921967137554702 ) ) ;
#17298 = LINE ( 'NONE', #2149, #9929 ) ;
#17299 = EDGE_CURVE ( 'NONE', #12008, #5370, #7301, .T. ) ;
#17300 = CIRCLE ( 'NONE', #11281, 9.999999999999998224 ) ;
#17301 = ORIENTED_EDGE ( 'NONE', *, *, #4247, .F. ) ;
#17302 = DIRECTION ( 'NONE',  ( 0.000000000000000000, 0.8987940462991651502, 0.4383711467890813451 ) ) ;
#17303 = ORIENTED_EDGE ( 'NONE', *, *, #21619, .F. ) ;
#17304 = DIRECTION ( 'NONE',  ( 0.000000000000000000, 0.000000000000000000, 1.000000000000000000 ) ) ;
#17305 = ADVANCED_FACE ( 'NONE', ( #6981 ), #10380, .F. ) ;
#17306 = ORIENTED_EDGE ( 'NONE', *, *, #1379, .T. ) ;
#17307 = DIRECTION ( 'NONE',  ( -1.000000000000000000, 0.000000000000000000, -0.000000000000000000 ) ) ;
#17308 = LINE ( 'NONE', #19068, #1742 ) ;
#17309 = VERTEX_POINT ( 'NONE', #14026 ) ;
#17310 = EDGE_CURVE ( 'NONE', #14140, #13603, #7990, .T. ) ;
#17311 = VERTEX_POINT ( 'NONE', #5423 ) ;
#17312 = ORIENTED_EDGE ( 'NONE', *, *, #20574, .F. ) ;
#17313 = ORIENTED_EDGE ( 'NONE', *, *, #10714, .T. ) ;
#17314 = AXIS2_PLACEMENT_3D ( 'NONE', #11512, #18586, #3442 ) ;
#17315 = DIRECTION ( 'NONE',  ( -1.000000000000000000, -0.000000000000000000, 0.000000000000000000 ) ) ;
#17316 = ORIENTED_EDGE ( 'NONE', *, *, #16988, .F. ) ;
#17317 = DIRECTION ( 'NONE',  ( 1.000000000000000000, 0.000000000000000000, 0.000000000000000000 ) ) ;
#17318 = CARTESIAN_POINT ( 'NONE',  ( 10.00000000000000000, -17.83210509884626660, -21.83428559348779530 ) ) ;
#17319 = CYLINDRICAL_SURFACE ( 'NONE', #3709, 88.00000000000000000 ) ;
#17320 = EDGE_CURVE ( 'NONE', #2139, #14884, #10087, .T. ) ;
#17321 = DIRECTION ( 'NONE',  ( 0.000000000000000000, 0.000000000000000000, 1.000000000000000000 ) ) ;
#17322 = LINE ( 'NONE', #5383, #7478 ) ;
#17323 = EDGE_CURVE ( 'NONE', #2849, #4329, #3401, .T. ) ;
#17324 = CARTESIAN_POINT ( 'NONE',  ( 10.00000000000000000, 61.33825423015685629, 69.23910433415966281 ) ) ;
#17325 = ORIENTED_EDGE ( 'NONE', *, *, #11893, .F. ) ;
#17326 = LINE ( 'NONE', #5501, #4216 ) ;
#17327 = DIRECTION ( 'NONE',  ( -1.000000000000000000, 0.000000000000000000, -0.000000000000000000 ) ) ;
#17328 = VECTOR ( 'NONE', #20561, 1000.000000000000000 ) ;
#17329 = DIRECTION ( 'NONE',  ( 0.000000000000000000, 1.680754301168640043E-14, -1.000000000000000000 ) ) ;
#17330 = ADVANCED_FACE ( 'NONE', ( #12150 ), #15794, .T. ) ;
#17331 = ORIENTED_EDGE ( 'NONE', *, *, #14224, .T. ) ;
#17332 = DIRECTION ( 'NONE',  ( 0.000000000000000000, 0.000000000000000000, 1.000000000000000000 ) ) ;
#17333 = VERTEX_POINT ( 'NONE', #17246 ) ;
#17334 = DIRECTION ( 'NONE',  ( -1.000000000000000000, 0.000000000000000000, 0.000000000000000000 ) ) ;
#17335 = EDGE_CURVE ( 'NONE', #14552, #18616, #17867, .T. ) ;
#17336 = ORIENTED_EDGE ( 'NONE', *, *, #6673, .T. ) ;
#17337 = VERTEX_POINT ( 'NONE', #3759 ) ;
#17338 = ADVANCED_FACE ( 'NONE', ( #1879 ), #2315, .T. ) ;
#17339 = CARTESIAN_POINT ( 'NONE',  ( 0.000000000000000000, 23.10190250628953379, -89.56973317806578905 ) ) ;
#17340 = EDGE_CURVE ( 'NONE', #1609, #9924, #2111, .T. ) ;
#17341 = ORIENTED_EDGE ( 'NONE', *, *, #1587, .T. ) ;
#17342 = DIRECTION ( 'NONE',  ( 0.000000000000000000, 0.000000000000000000, -1.000000000000000000 ) ) ;
#17343 = CARTESIAN_POINT ( 'NONE',  ( 10.00000000000000000, 27.00677879429026618, 80.65868421664441712 ) ) ;
#17344 = DIRECTION ( 'NONE',  ( 1.000000000000000000, 0.000000000000000000, 0.000000000000000000 ) ) ;
#17345 = DIRECTION ( 'NONE',  ( 0.000000000000000000, 0.000000000000000000, 1.000000000000000000 ) ) ;
#17346 = FACE_OUTER_BOUND ( 'NONE', #10915, .T. ) ;
#17347 = ADVANCED_FACE ( 'NONE', ( #15578 ), #7185, .T. ) ;
#17348 = CARTESIAN_POINT ( 'NONE',  ( 0.000000000000000000, -11.59241532900569993, -87.23311244498751194 ) ) ;
#17349 = DIRECTION ( 'NONE',  ( 0.000000000000000000, 0.000000000000000000, 1.000000000000000000 ) ) ;
#17350 = DIRECTION ( 'NONE',  ( 0.000000000000000000, 0.4067366430757948237, 0.9135454576426033091 ) ) ;
#17351 = DIRECTION ( 'NONE',  ( 1.000000000000000000, 0.000000000000000000, 0.000000000000000000 ) ) ;
#17352 = ORIENTED_EDGE ( 'NONE', *, *, #20341, .F. ) ;
#17353 = DIRECTION ( 'NONE',  ( 0.000000000000000000, -0.8660254037844432595, 0.4999999999999919509 ) ) ;
#17354 = ORIENTED_EDGE ( 'NONE', *, *, #3089, .F. ) ;
#17355 = STYLED_ITEM ( 'NONE', ( #16955 ), #5094 ) ;
#17356 = ORIENTED_EDGE ( 'NONE', *, *, #4206, .F. ) ;
#17357 = VERTEX_POINT ( 'NONE', #3873 ) ;
#17358 = DIRECTION ( 'NONE',  ( 0.000000000000000000, 0.000000000000000000, -1.000000000000000000 ) ) ;
#17359 = ORIENTED_EDGE ( 'NONE', *, *, #8034, .F. ) ;
#17360 = ORIENTED_EDGE ( 'NONE', *, *, #11742, .F. ) ;
#17361 = EDGE_CURVE ( 'NONE', #13595, #13159, #4819, .T. ) ;
#17362 = CARTESIAN_POINT ( 'NONE',  ( 5.000000000000000000, 28.00896854771991329, 15.47571261340933724 ) ) ;
#17363 = ORIENTED_EDGE ( 'NONE', *, *, #19051, .F. ) ;
#17364 = CARTESIAN_POINT ( 'NONE',  ( 1.399999999999998579, 6.123233995736766282E-16, 5.000000000000000000 ) ) ;
#17365 = CARTESIAN_POINT ( 'NONE',  ( 10.00000000000000000, 0.000000000000000000, 0.000000000000000000 ) ) ;
#17366 = DIRECTION ( 'NONE',  ( -1.000000000000000000, 0.000000000000000000, 0.000000000000000000 ) ) ;
#17367 = DIRECTION ( 'NONE',  ( -1.000000000000000000, 0.000000000000000000, 0.000000000000000000 ) ) ;
#17368 = DIRECTION ( 'NONE',  ( -1.000000000000000000, 0.000000000000000000, -0.000000000000000000 ) ) ;
#17369 = DIRECTION ( 'NONE',  ( -1.000000000000000000, -0.000000000000000000, -0.000000000000000000 ) ) ;
#17370 = FACE_OUTER_BOUND ( 'NONE', #8603, .T. ) ;
#17371 = DIRECTION ( 'NONE',  ( -1.000000000000000000, 0.000000000000000000, 0.000000000000000000 ) ) ;
#17372 = AXIS2_PLACEMENT_3D ( 'NONE', #11374, #19784, #14693 ) ;
#17373 = VERTEX_POINT ( 'NONE', #20874 ) ;
#17374 = VECTOR ( 'NONE', #7745, 1000.000000000000000 ) ;
#17375 = LINE ( 'NONE', #5774, #20072 ) ;
#17376 = CARTESIAN_POINT ( 'NONE',  ( -7.600000000000002309, 0.000000000000000000, 0.000000000000000000 ) ) ;
#17377 = ORIENTED_EDGE ( 'NONE', *, *, #14328, .F. ) ;
#17378 = ADVANCED_FACE ( 'NONE', ( #5747 ), #12472, .F. ) ;
#17379 = CARTESIAN_POINT ( 'NONE',  ( 5.000000000000000000, 30.71797041605808687, 82.46457599186561538 ) ) ;
#17380 = ORIENTED_EDGE ( 'NONE', *, *, #13640, .F. ) ;
#17381 =( NAMED_UNIT ( * ) PLANE_ANGLE_UNIT ( ) SI_UNIT ( $, .RADIAN. ) );
#17382 = FACE_OUTER_BOUND ( 'NONE', #19842, .T. ) ;
#17383 = CIRCLE ( 'NONE', #1514, 88.00000000000000000 ) ;
#17384 = ORIENTED_EDGE ( 'NONE', *, *, #21369, .F. ) ;
#17385 = EDGE_LOOP ( 'NONE', ( #19298, #5296, #20297, #16338 ) ) ;
#17386 = FACE_OUTER_BOUND ( 'NONE', #8992, .T. ) ;
#17387 = CARTESIAN_POINT ( 'NONE',  ( 126.5000000000000000, 0.000000000000000000, 25.00000000000000000 ) ) ;
#17388 = PRODUCT_RELATED_PRODUCT_CATEGORY ( 'part', '', ( #18138 ) ) ;
#17389 = AXIS2_PLACEMENT_3D ( 'NONE', #16018, #7635, #14372 ) ;
#17390 = CIRCLE ( 'NONE', #2919, 88.00000000000000000 ) ;
#17391 = DIRECTION ( 'NONE',  ( 0.000000000000000000, 0.000000000000000000, 1.000000000000000000 ) ) ;
#17392 = CARTESIAN_POINT ( 'NONE',  ( -1.500000000000000000, 0.000000000000000000, 5.000000000000000000 ) ) ;
#17393 = DIRECTION ( 'NONE',  ( 0.000000000000000000, 0.000000000000000000, -1.000000000000000000 ) ) ;
#17394 = DIRECTION ( 'NONE',  ( 1.000000000000000000, 0.000000000000000000, 0.000000000000000000 ) ) ;
#17395 = AXIS2_PLACEMENT_3D ( 'NONE', #12117, #15323, #13996 ) ;
#17396 = LINE ( 'NONE', #4244, #21310 ) ;
#17397 = DIRECTION ( 'NONE',  ( -1.000000000000000000, 0.000000000000000000, 0.000000000000000000 ) ) ;
#17398 = CIRCLE ( 'NONE', #6826, 123.0000000000000000 ) ;
#17399 = EDGE_LOOP ( 'NONE', ( #19092, #14706, #17727, #16689 ) ) ;
#17400 = DIRECTION ( 'NONE',  ( 1.000000000000000000, 0.000000000000000000, 0.000000000000000000 ) ) ;
#17401 = CIRCLE ( 'NONE', #7873, 88.00000000000000000 ) ;
#17402 = VERTEX_POINT ( 'NONE', #1203 ) ;
#17403 = CARTESIAN_POINT ( 'NONE',  ( 1.114299999999999846, 0.000000000000000000, 0.000000000000000000 ) ) ;
#17404 = ORIENTED_EDGE ( 'NONE', *, *, #7088, .F. ) ;
#17405 = AXIS2_PLACEMENT_3D ( 'NONE', #7236, #9200, #3914 ) ;
#17406 = DIRECTION ( 'NONE',  ( 0.000000000000000000, 0.4067366430758008744, -0.9135454576426006446 ) ) ;
#17407 = EDGE_CURVE ( 'NONE', #659, #13715, #21042, .T. ) ;
#17408 = DIRECTION ( 'NONE',  ( 0.000000000000000000, 0.000000000000000000, -1.000000000000000000 ) ) ;
#17409 = ORIENTED_EDGE ( 'NONE', *, *, #567, .F. ) ;
#17410 = AXIS2_PLACEMENT_3D ( 'NONE', #8453, #15177, #13517 ) ;
#17411 = EDGE_LOOP ( 'NONE', ( #6727, #13272, #17028, #10031 ) ) ;
#17412 = VERTEX_POINT ( 'NONE', #15904 ) ;
#17413 = ORIENTED_EDGE ( 'NONE', *, *, #17949, .F. ) ;
#17414 = PLANE ( 'NONE',  #12133 ) ;
#17415 = EDGE_LOOP ( 'NONE', ( #3897, #559, #4365, #9159 ) ) ;
#17416 = CIRCLE ( 'NONE', #2580, 5.100000000000000533 ) ;
#17417 = CARTESIAN_POINT ( 'NONE',  ( 10.00000000000000000, -87.96697768756403946, 2.410567674970269358 ) ) ;
#17418 = LINE ( 'NONE', #1846, #14035 ) ;
#17419 = DIRECTION ( 'NONE',  ( 1.000000000000000000, 0.000000000000000000, 0.000000000000000000 ) ) ;
#17420 = CARTESIAN_POINT ( 'NONE',  ( 0.000000000000000000, 9.992993448021589842, 26.36019881529889020 ) ) ;
#17421 = DIRECTION ( 'NONE',  ( 1.000000000000000000, 0.000000000000000000, 0.000000000000000000 ) ) ;
#17422 = EDGE_CURVE ( 'NONE', #733, #9395, #2639, .T. ) ;
#17423 = CIRCLE ( 'NONE', #9639, 44.99999999999999289 ) ;
#17424 = FACE_OUTER_BOUND ( 'NONE', #1403, .T. ) ;
#17425 = VERTEX_POINT ( 'NONE', #872 ) ;
#17426 = VECTOR ( 'NONE', #2165, 1000.000000000000000 ) ;
#17427 = EDGE_CURVE ( 'NONE', #20567, #8545, #7637, .T. ) ;
#17428 = DIRECTION ( 'NONE',  ( 0.000000000000000000, 0.000000000000000000, -1.000000000000000000 ) ) ;
#17429 = CARTESIAN_POINT ( 'NONE',  ( 10.00000000000000000, 0.000000000000000000, 0.000000000000000000 ) ) ;
#17430 = CARTESIAN_POINT ( 'NONE',  ( 10.00000000000000000, 0.000000000000000000, 0.000000000000000000 ) ) ;
#17431 = VERTEX_POINT ( 'NONE', #7732 ) ;
#17432 = AXIS2_PLACEMENT_3D ( 'NONE', #626, #12656, #2603 ) ;
#17433 = ADVANCED_FACE ( 'NONE', ( #2424 ), #12585, .T. ) ;
#17434 = CARTESIAN_POINT ( 'NONE',  ( 0.000000000000000000, 0.000000000000000000, 0.000000000000000000 ) ) ;
#17435 = EDGE_CURVE ( 'NONE', #18093, #6084, #909, .T. ) ;
#17436 = ADVANCED_FACE ( 'NONE', ( #18014, #12695 ), #21208, .T. ) ;
#17437 = EDGE_LOOP ( 'NONE', ( #11136, #3307, #3714, #17089 ) ) ;
#17438 = CARTESIAN_POINT ( 'NONE',  ( -123.0000000000000000, 1.506315562951244531E-14, 25.00000000000000000 ) ) ;
#17439 = ORIENTED_EDGE ( 'NONE', *, *, #21201, .T. ) ;
#17440 = CIRCLE ( 'NONE', #2620, 88.00000000000000000 ) ;
#17441 = EDGE_CURVE ( 'NONE', #4912, #12422, #19330, .T. ) ;
#17442 = ORIENTED_EDGE ( 'NONE', *, *, #18164, .F. ) ;
#17443 = ORIENTED_EDGE ( 'NONE', *, *, #20020, .T. ) ;
#17444 = DIRECTION ( 'NONE',  ( 0.000000000000000000, 0.5877852522924689183, 0.8090169943749504489 ) ) ;
#17445 = VECTOR ( 'NONE', #20164, 1000.000000000000000 ) ;
#17446 = ORIENTED_EDGE ( 'NONE', *, *, #13009, .F. ) ;
#17447 = CARTESIAN_POINT ( 'NONE',  ( 0.000000000000000000, -61.60362715318993310, -62.84101464466307618 ) ) ;
#17448 = EDGE_CURVE ( 'NONE', #1558, #9557, #3065, .T. ) ;
#17449 = LINE ( 'NONE', #11020, #871 ) ;
#17450 = DIRECTION ( 'NONE',  ( 0.000000000000000000, 0.9510565162951544194, -0.3090169943749450643 ) ) ;
#17451 = CARTESIAN_POINT ( 'NONE',  ( 0.000000000000000000, 0.000000000000000000, 0.000000000000000000 ) ) ;
#17452 = ADVANCED_FACE ( 'NONE', ( #7507 ), #14566, .F. ) ;
#17453 = AXIS2_PLACEMENT_3D ( 'NONE', #5470, #10540, #15616 ) ;
#17454 = DIRECTION ( 'NONE',  ( -1.000000000000000000, -0.000000000000000000, 0.000000000000000000 ) ) ;
#17455 = CARTESIAN_POINT ( 'NONE',  ( 0.000000000000000000, 15.00000000000000000, 0.000000000000000000 ) ) ;
#17456 = CARTESIAN_POINT ( 'NONE',  ( 0.000000000000000000, -9.992993448021419312, -26.36019881529895770 ) ) ;
#17457 = CARTESIAN_POINT ( 'NONE',  ( 7.395799999999999486, 1.287093988729475069E-14, 105.0992000000000104 ) ) ;
#17458 = EDGE_CURVE ( 'NONE', #6503, #21168, #15406, .T. ) ;
#17459 = CARTESIAN_POINT ( 'NONE',  ( 10.00000000000000000, 30.71797041605924505, -82.46457599186518905 ) ) ;
#17460 = AXIS2_PLACEMENT_3D ( 'NONE', #10747, #15732, #3906 ) ;
#17461 = ORIENTED_EDGE ( 'NONE', *, *, #445, .T. ) ;
#17462 = AXIS2_PLACEMENT_3D ( 'NONE', #15610, #12620, #17176 ) ;
#17463 = ADVANCED_FACE ( 'NONE', ( #19771 ), #4634, .F. ) ;
#17464 = DIRECTION ( 'NONE',  ( 0.000000000000000000, 0.000000000000000000, -1.000000000000000000 ) ) ;
#17465 = ORIENTED_EDGE ( 'NONE', *, *, #20629, .F. ) ;
#17466 = EDGE_LOOP ( 'NONE', ( #19836, #2269, #20269, #16902 ) ) ;
#17467 = EDGE_LOOP ( 'NONE', ( #613, #2489, #9057, #16144 ) ) ;
#17468 = DIRECTION ( 'NONE',  ( 0.000000000000000000, -0.5299192642331944647, -0.8480480961564325071 ) ) ;
#17469 = VECTOR ( 'NONE', #6241, 1000.000000000000000 ) ;
#17470 = ADVANCED_FACE ( 'NONE', ( #7618 ), #4197, .F. ) ;
#17471 = EDGE_LOOP ( 'NONE', ( #5422, #7060, #12331, #673, #3576, #3035, #21403, #1175, #18650, #2704, #18084, #19271, #18001, #3502, #12355, #13800, #21245, #3194, #1155, #1723, #21698, #21525, #444, #2150, #2530, #16723, #10151, #676, #17655, #19498, #14821, #3280, #11753, #13760, #15223, #3195, #19667, #18456, #10522, #11566, #9427, #21774, #21389, #15207, #1215, #14949, #2866, #12222, #12446, #13646, #11597, #11390, #8579, #8479, #13131, #15081, #8528, #3052, #9816, #12471, #12328, #4639, #17963, #6852, #16073, #4510, #20992, #1568, #2048, #10054, #10828, #5092, #4921, #21807, #13455, #7470, #16512, #7914, #7276, #18020, #2727, #2800, #5349, #2995, #9166, #21051, #20515, #19932, #4162, #12351, #17198, #13921, #8496, #20517, #14664, #12046, #6371, #20068, #19414, #20535, #8365, #20955, #5171, #14524, #1951, #8841, #18613, #21445, #14434, #10123, #19094, #3088, #11285, #4478, #7696, #10181, #2265, #6664, #15218, #6015, #8392, #565, #21732, #9214, #20969, #16236, #11244, #93, #19226, #20186, #20591, #19195, #2546, #3977, #18798, #20469, #768, #8117, #16269, #20862, #15256, #20190, #1954, #3446, #4221, #13046, #7480, #19972, #20083, #19471, #15477, #18802, #21465, #12327, #11809, #7492, #11151, #1277, #8796, #214, #14505, #5696, #14109, #15693, #3162, #9261, #16810, #18708, #12239, #19759, #7715, #4919, #11287, #16238, #18397, #16461, #20501, #4475, #20942, #7918, #11946, #18580, #19822, #9995, #1474, #21696, #11309, #5652, #15980, #11270, #14532, #10906, #13576, #4499, #6291, #12480, #15429, #875, #17986, #1018, #13442, #14744, #12593, #14305, #9494, #21604, #1534, #18, #21839, #349, #7113, #14579, #13034, #4301, #15556, #11972, #16089, #15986, #16836, #4950, #10093, #7372, #10452, #16900, #7368, #11269, #11887, #2920, #507, #15873, #3757, #20159, #17515, #17115, #9454, #10415, #7535, #14641, #17046, #3063, #21039, #11997, #15178, #21139, #10588, #10995, #640, #6753, #18238, #6817, #16402, #18741, #6172, #16870, #12801, #9210, #17380, #20904, #10096, #20590, #6169, #16367, #20411, #16546, #1820, #18682, #13432, #19309, #14748, #6798, #21687, #5161, #3212, #12152, #10761, #14425, #18372, #15250, #10284, #7839, #3571, #16696, #3364, #15797, #6038, #17709, #4796, #9237, #2673, #7016, #5689, #20114, #19580, #10555, #1764, #10854, #5976, #9051, #21261, #21144, #16362, #20016, #11634, #9372, #2784, #7287, #18096, #12947, #10225, #20726, #20239, #1682, #15331, #14568, #3766, #14304, #13351, #13216, #14666, #11683, #19284, #4740, #322, #12731, #17578, #18963, #12193, #12675, #15439, #3995, #6001, #11515, #18585, #1228, #16341, #12506, #2703, #14094, #9158, #14139, #11841, #18990, #5650, #20779, #8278, #19387, #5460, #79, #4453, #12344, #19816, #7393, #10801, #12895, #2407, #4031, #15201, #5755, #18871, #7627, #20132, #20129, #17000 ) ) ;
#17472 = ORIENTED_EDGE ( 'NONE', *, *, #20175, .T. ) ;
#17473 = AXIS2_PLACEMENT_3D ( 'NONE', #1306, #21622, #17885 ) ;
#17474 = ORIENTED_EDGE ( 'NONE', *, *, #4236, .F. ) ;
#17475 = CIRCLE ( 'NONE', #20301, 118.9000000000000199 ) ;
#17476 = DIRECTION ( 'NONE',  ( 0.000000000000000000, 1.000000000000000000, -1.224646799147353207E-16 ) ) ;
#17477 = ORIENTED_EDGE ( 'NONE', *, *, #13915, .F. ) ;
#17478 = CARTESIAN_POINT ( 'NONE',  ( 10.00000000000000000, 61.60362715319035942, 62.84101464466265696 ) ) ;
#17479 = CARTESIAN_POINT ( 'NONE',  ( 10.00000000000000000, 91.70173545986517638, 12.13370160540072362 ) ) ;
#17480 = CARTESIAN_POINT ( 'NONE',  ( 0.000000000000000000, 90.63195040374188238, 18.50093422002450083 ) ) ;
#17481 = DIRECTION ( 'NONE',  ( 0.000000000000000000, 0.000000000000000000, 1.000000000000000000 ) ) ;
#17482 = DIRECTION ( 'NONE',  ( 0.000000000000000000, 0.000000000000000000, 1.000000000000000000 ) ) ;
#17483 = ADVANCED_FACE ( 'NONE', ( #1095 ), #17677, .F. ) ;
#17484 = DIRECTION ( 'NONE',  ( -1.000000000000000000, 0.000000000000000000, -0.000000000000000000 ) ) ;
#17485 = DIRECTION ( 'NONE',  ( 0.000000000000000000, 0.4694715627858917495, -0.8829475928589264333 ) ) ;
#17486 = LINE ( 'NONE', #17921, #21131 ) ;
#17487 = CIRCLE ( 'NONE', #10763, 11.99999999999999822 ) ;
#17488 = CIRCLE ( 'NONE', #4073, 32.00000000000000000 ) ;
#17489 = EDGE_CURVE ( 'NONE', #17903, #1766, #7651, .T. ) ;
#17490 = VERTEX_POINT ( 'NONE', #16122 ) ;
#17491 = CIRCLE ( 'NONE', #4074, 92.50100000000000477 ) ;
#17492 = CIRCLE ( 'NONE', #4768, 88.00000000000000000 ) ;
#17493 = EDGE_CURVE ( 'NONE', #12744, #21233, #5188, .T. ) ;
#17494 = DIRECTION ( 'NONE',  ( 0.000000000000000000, 0.000000000000000000, 1.000000000000000000 ) ) ;
#17495 = AXIS2_PLACEMENT_3D ( 'NONE', #3885, #21005, #9170 ) ;
#17496 = DIRECTION ( 'NONE',  ( -1.000000000000000000, 0.000000000000000000, -0.000000000000000000 ) ) ;
#17497 = DIRECTION ( 'NONE',  ( 1.000000000000000000, 0.000000000000000000, 0.000000000000000000 ) ) ;
#17498 = VERTEX_POINT ( 'NONE', #15008 ) ;
#17499 = LINE ( 'NONE', #2349, #5592 ) ;
#17500 = EDGE_LOOP ( 'NONE', ( #16376, #17325, #4549, #21266 ) ) ;
#17501 = DIRECTION ( 'NONE',  ( 0.000000000000000000, 0.8987940462991649282, 0.4383711467890815117 ) ) ;
#17502 = ORIENTED_EDGE ( 'NONE', *, *, #2972, .T. ) ;
#17503 = AXIS2_PLACEMENT_3D ( 'NONE', #18034, #9280, #1341 ) ;
#17504 = ORIENTED_EDGE ( 'NONE', *, *, #3423, .F. ) ;
#17505 = DIRECTION ( 'NONE',  ( 0.000000000000000000, 0.000000000000000000, 1.000000000000000000 ) ) ;
#17506 = CIRCLE ( 'NONE', #7971, 44.99999999999999289 ) ;
#17507 = CIRCLE ( 'NONE', #2667, 100.0000000000000000 ) ;
#17508 = DIRECTION ( 'NONE',  ( 0.000000000000000000, -0.2756373558169870064, -0.9612616959383222248 ) ) ;
#17509 = DIRECTION ( 'NONE',  ( 1.000000000000000000, 0.000000000000000000, 0.000000000000000000 ) ) ;
#17510 = CARTESIAN_POINT ( 'NONE',  ( 10.00000000000000000, 48.19312842678564834, -70.09002648625148879 ) ) ;
#17511 = CARTESIAN_POINT ( 'NONE',  ( 0.000000000000000000, -84.12297548659729785, 12.59025161326973397 ) ) ;
#17512 = FACE_OUTER_BOUND ( 'NONE', #16828, .T. ) ;
#17513 = DIRECTION ( 'NONE',  ( 0.000000000000000000, 0.000000000000000000, -1.000000000000000000 ) ) ;
#17514 = DIRECTION ( 'NONE',  ( -1.000000000000000000, -0.000000000000000000, 0.000000000000000000 ) ) ;
#17515 = ORIENTED_EDGE ( 'NONE', *, *, #5533, .F. ) ;
#17516 = FACE_OUTER_BOUND ( 'NONE', #180, .T. ) ;
#17517 = ORIENTED_EDGE ( 'NONE', *, *, #8163, .T. ) ;
#17518 = VECTOR ( 'NONE', #18901, 1000.000000000000000 ) ;
#17519 = CIRCLE ( 'NONE', #15743, 10.49999999999999822 ) ;
#17520 = CARTESIAN_POINT ( 'NONE',  ( -8.900000000000012790, 0.000000000000000000, 0.000000000000000000 ) ) ;
#17521 = VERTEX_POINT ( 'NONE', #19872 ) ;
#17522 = PLANE ( 'NONE',  #15139 ) ;
#17523 = DIRECTION ( 'NONE',  ( -1.000000000000000000, 0.000000000000000000, 0.000000000000000000 ) ) ;
#17524 = ORIENTED_EDGE ( 'NONE', *, *, #4869, .F. ) ;
#17525 = ORIENTED_EDGE ( 'NONE', *, *, #21081, .F. ) ;
#17526 = VERTEX_POINT ( 'NONE', #3412 ) ;
#17527 = ORIENTED_EDGE ( 'NONE', *, *, #3518, .F. ) ;
#17528 = DIRECTION ( 'NONE',  ( 0.000000000000000000, 0.2756373558169932236, 0.9612616959383206705 ) ) ;
#17529 = DIRECTION ( 'NONE',  ( 1.000000000000000000, 0.000000000000000000, 0.000000000000000000 ) ) ;
#17530 = ORIENTED_EDGE ( 'NONE', *, *, #8506, .F. ) ;
#17531 = AXIS2_PLACEMENT_3D ( 'NONE', #9986, #8345, #6710 ) ;
#17532 = CARTESIAN_POINT ( 'NONE',  ( 10.00000000000000000, -61.33825423015638734, -69.23910433416007493 ) ) ;
#17533 = CARTESIAN_POINT ( 'NONE',  ( 10.00000000000000000, 21.98203405400955290, 17.64965094506551324 ) ) ;
#17534 = AXIS2_PLACEMENT_3D ( 'NONE', #13889, #10468, #15555 ) ;
#17535 = LINE ( 'NONE', #2387, #5484 ) ;
#17536 = DIRECTION ( 'NONE',  ( -1.000000000000000000, -0.000000000000000000, -0.000000000000000000 ) ) ;
#17537 = AXIS2_PLACEMENT_3D ( 'NONE', #12926, #1337, #6541 ) ;
#17538 = CYLINDRICAL_SURFACE ( 'NONE', #15388, 113.8250000000000028 ) ;
#17539 = EDGE_CURVE ( 'NONE', #2562, #9461, #1304, .T. ) ;
#17540 = EDGE_LOOP ( 'NONE', ( #11172, #6564, #6746, #12103 ) ) ;
#17541 = CARTESIAN_POINT ( 'NONE',  ( 10.00000000000000000, 46.07110168784925008, -74.97635353408335845 ) ) ;
#17542 = LINE ( 'NONE', #9448, #19938 ) ;
#17543 = EDGE_CURVE ( 'NONE', #2613, #3811, #6960, .T. ) ;
#17544 = CARTESIAN_POINT ( 'NONE',  ( -1.200000000000006617, 0.000000000000000000, -5.612499999999999822 ) ) ;
#17545 = ORIENTED_EDGE ( 'NONE', *, *, #17, .F. ) ;
#17546 = DIRECTION ( 'NONE',  ( 1.000000000000000000, 0.000000000000000000, 0.000000000000000000 ) ) ;
#17547 = AXIS2_PLACEMENT_3D ( 'NONE', #3521, #3946, #5183 ) ;
#17548 = ORIENTED_EDGE ( 'NONE', *, *, #8650, .T. ) ;
#17549 = DIRECTION ( 'NONE',  ( -1.000000000000000000, -0.000000000000000000, -0.000000000000000000 ) ) ;
#17550 = CIRCLE ( 'NONE', #8026, 44.99999999999998579 ) ;
#17551 = ORIENTED_EDGE ( 'NONE', *, *, #2788, .T. ) ;
#17552 = EDGE_LOOP ( 'NONE', ( #7771, #13862, #2095, #21838 ) ) ;
#17553 = VERTEX_POINT ( 'NONE', #18446 ) ;
#17554 = CARTESIAN_POINT ( 'NONE',  ( 10.00000000000000000, -28.15804365424196121, -1.358152127006266197 ) ) ;
#17555 = ORIENTED_EDGE ( 'NONE', *, *, #12448, .F. ) ;
#17556 = CARTESIAN_POINT ( 'NONE',  ( 0.000000000000000000, -87.92084725184950855, 3.731570516142653116 ) ) ;
#17557 = LINE ( 'NONE', #12781, #18173 ) ;
#17558 = FACE_OUTER_BOUND ( 'NONE', #2186, .T. ) ;
#17559 = CARTESIAN_POINT ( 'NONE',  ( 10.00000000000000000, 27.00677879429135331, -80.65868421664406185 ) ) ;
#17560 = VECTOR ( 'NONE', #9220, 1000.000000000000000 ) ;
#17561 = CYLINDRICAL_SURFACE ( 'NONE', #6822, 45.00000000000000000 ) ;
#17562 = EDGE_CURVE ( 'NONE', #10277, #6346, #20697, .T. ) ;
#17563 = DIRECTION ( 'NONE',  ( 0.000000000000000000, -0.9848077530122062440, -0.1736481776669404620 ) ) ;
#17564 = ADVANCED_FACE ( 'NONE', ( #6632 ), #14697, .T. ) ;
#17565 = DIRECTION ( 'NONE',  ( 1.000000000000000000, -0.000000000000000000, 0.000000000000000000 ) ) ;
#17566 = EDGE_CURVE ( 'NONE', #7709, #17245, #21753, .T. ) ;
#17567 = AXIS2_PLACEMENT_3D ( 'NONE', #1144, #7667, #17834 ) ;
#17568 = VECTOR ( 'NONE', #9917, 1000.000000000000000 ) ;
#17569 = CARTESIAN_POINT ( 'NONE',  ( 10.00000000000000000, 85.05652083079334602, 0.7600687895874258526 ) ) ;
#17570 = DIRECTION ( 'NONE',  ( -1.000000000000000000, 0.000000000000000000, -0.000000000000000000 ) ) ;
#17571 = EDGE_CURVE ( 'NONE', #419, #18142, #2695, .T. ) ;
#17572 = DIRECTION ( 'NONE',  ( -1.000000000000000000, -0.000000000000000000, -0.000000000000000000 ) ) ;
#17573 = ORIENTED_EDGE ( 'NONE', *, *, #19637, .F. ) ;
#17574 = ORIENTED_EDGE ( 'NONE', *, *, #14313, .T. ) ;
#17575 = ORIENTED_EDGE ( 'NONE', *, *, #12584, .T. ) ;
#17576 = EDGE_CURVE ( 'NONE', #3283, #13187, #11166, .T. ) ;
#17577 = AXIS2_PLACEMENT_3D ( 'NONE', #5330, #15697, #5220 ) ;
#17578 = ORIENTED_EDGE ( 'NONE', *, *, #4607, .F. ) ;
#17579 = VECTOR ( 'NONE', #18492, 1000.000000000000000 ) ;
#17580 = CIRCLE ( 'NONE', #11589, 44.99999999999999289 ) ;
#17581 = ORIENTED_EDGE ( 'NONE', *, *, #3952, .F. ) ;
#17582 = EDGE_CURVE ( 'NONE', #6657, #17054, #948, .T. ) ;
#17583 = DIRECTION ( 'NONE',  ( 0.000000000000000000, 0.000000000000000000, 1.000000000000000000 ) ) ;
#17584 = ORIENTED_EDGE ( 'NONE', *, *, #170, .F. ) ;
#17585 = CARTESIAN_POINT ( 'NONE',  ( 1.500000000000000000, -7.000000000000000000, 5.000000000000000000 ) ) ;
#17586 = CARTESIAN_POINT ( 'NONE',  ( 10.00000000000000000, 0.000000000000000000, 0.000000000000000000 ) ) ;
#17587 = DIRECTION ( 'NONE',  ( 1.000000000000000000, 0.000000000000000000, 0.000000000000000000 ) ) ;
#17588 = DIRECTION ( 'NONE',  ( -1.000000000000000000, 0.000000000000000000, 0.000000000000000000 ) ) ;
#17589 = DIRECTION ( 'NONE',  ( 0.000000000000000000, 0.7431448254773953543, -0.6691306063588569053 ) ) ;
#17590 = DIRECTION ( 'NONE',  ( -1.000000000000000000, -0.000000000000000000, 0.000000000000000000 ) ) ;
#17591 = CARTESIAN_POINT ( 'NONE',  ( 0.000000000000000000, 0.000000000000000000, 0.000000000000000000 ) ) ;
#17592 = CARTESIAN_POINT ( 'NONE',  ( 10.00000000000000000, -65.83713140174687339, -58.39068529131263574 ) ) ;
#17593 = AXIS2_PLACEMENT_3D ( 'NONE', #11815, #2, #13036 ) ;
#17594 = ADVANCED_FACE ( 'NONE', ( #1753 ), #1432, .F. ) ;
#17595 = VECTOR ( 'NONE', #17334, 1000.000000000000000 ) ;
#17596 = VECTOR ( 'NONE', #18670, 1000.000000000000000 ) ;
#17597 = EDGE_LOOP ( 'NONE', ( #9972, #15869, #15639, #12918 ) ) ;
#17598 = AXIS2_PLACEMENT_3D ( 'NONE', #19455, #4314, #7758 ) ;
#17599 = CARTESIAN_POINT ( 'NONE',  ( 0.000000000000000000, 0.000000000000000000, 0.000000000000000000 ) ) ;
#17600 = CARTESIAN_POINT ( 'NONE',  ( -1.200000000000006617, 0.000000000000000000, -6.887500000000022382 ) ) ;
#17601 = ADVANCED_FACE ( 'NONE', ( #8171 ), #17005, .F. ) ;
#17602 = DIRECTION ( 'NONE',  ( -1.000000000000000000, -0.000000000000000000, -0.000000000000000000 ) ) ;
#17603 = EDGE_LOOP ( 'NONE', ( #6529, #3236, #1208, #6825 ) ) ;
#17604 = AXIS2_PLACEMENT_3D ( 'NONE', #15763, #627, #14206 ) ;
#17605 = CARTESIAN_POINT ( 'NONE',  ( 5.000000000000002665, 46.07110168784925008, -74.97635353408335845 ) ) ;
#17606 = EDGE_CURVE ( 'NONE', #9724, #17660, #6249, .T. ) ;
#17607 = VERTEX_POINT ( 'NONE', #6844 ) ;
#17608 = AXIS2_PLACEMENT_3D ( 'NONE', #10479, #10364, #13578 ) ;
#17609 = LINE ( 'NONE', #14391, #15978 ) ;
#17610 = VERTEX_POINT ( 'NONE', #3299 ) ;
#17611 = AXIS2_PLACEMENT_3D ( 'NONE', #21288, #9347, #849 ) ;
#17612 = ORIENTED_EDGE ( 'NONE', *, *, #17164, .T. ) ;
#17613 = ADVANCED_FACE ( 'NONE', ( #13568 ), #18113, .F. ) ;
#17614 = DIRECTION ( 'NONE',  ( 0.000000000000000000, 0.000000000000000000, 1.000000000000000000 ) ) ;
#17615 = VECTOR ( 'NONE', #5837, 1000.000000000000000 ) ;
#17616 = CIRCLE ( 'NONE', #21831, 32.00000000000000000 ) ;
#17617 = DIRECTION ( 'NONE',  ( 0.000000000000000000, 0.000000000000000000, 1.000000000000000000 ) ) ;
#17618 = EDGE_CURVE ( 'NONE', #18973, #13033, #13293, .T. ) ;
#17619 = DIRECTION ( 'NONE',  ( -1.000000000000000000, -0.000000000000000000, -0.000000000000000000 ) ) ;
#17620 = CARTESIAN_POINT ( 'NONE',  ( 10.00000000000000000, -78.04699792498111321, -49.64978465107371619 ) ) ;
#17621 = CARTESIAN_POINT ( 'NONE',  ( 10.00000000000000000, -61.71252885873347793, -58.53847642588656441 ) ) ;
#17622 = DIRECTION ( 'NONE',  ( -1.000000000000000000, 0.000000000000000000, 0.000000000000000000 ) ) ;
#17623 = CARTESIAN_POINT ( 'NONE',  ( 10.00000000000000000, 56.35896156214949571, 73.34918167666329225 ) ) ;
#17624 = DIRECTION ( 'NONE',  ( 0.000000000000000000, 0.6946583704589934793, 0.7193398003386547446 ) ) ;
#17625 = LINE ( 'NONE', #21038, #19669 ) ;
#17626 = ORIENTED_EDGE ( 'NONE', *, *, #19340, .F. ) ;
#17627 = LINE ( 'NONE', #9105, #12903 ) ;
#17628 = CIRCLE ( 'NONE', #16567, 88.00000000000000000 ) ;
#17629 = AXIS2_PLACEMENT_3D ( 'NONE', #7895, #21048, #19166 ) ;
#17630 = ORIENTED_EDGE ( 'NONE', *, *, #6089, .F. ) ;
#17631 = VECTOR ( 'NONE', #1505, 1000.000000000000000 ) ;
#17632 = AXIS2_PLACEMENT_3D ( 'NONE', #15550, #6955, #1643 ) ;
#17633 = CARTESIAN_POINT ( 'NONE',  ( 0.000000000000000000, -78.01214607583776228, 33.90124636420084414 ) ) ;
#17634 = ORIENTED_EDGE ( 'NONE', *, *, #21501, .T. ) ;
#17635 = DIRECTION ( 'NONE',  ( 1.000000000000000000, 0.000000000000000000, -0.000000000000000000 ) ) ;
#17636 = CARTESIAN_POINT ( 'NONE',  ( 0.000000000000000000, -30.24235385705245349, 10.45944707835097098 ) ) ;
#17637 = VERTEX_POINT ( 'NONE', #16779 ) ;
#17638 = ORIENTED_EDGE ( 'NONE', *, *, #1699, .F. ) ;
#17639 = ORIENTED_EDGE ( 'NONE', *, *, #10450, .T. ) ;
#17640 = EDGE_LOOP ( 'NONE', ( #4483, #11704, #19660, #1599 ) ) ;
#17641 = CARTESIAN_POINT ( 'NONE',  ( 10.00000000000000000, 61.71252885873465033, -58.53847642588533517 ) ) ;
#17642 = DIRECTION ( 'NONE',  ( 1.000000000000000000, 0.000000000000000000, 0.000000000000000000 ) ) ;
#17643 = ORIENTED_EDGE ( 'NONE', *, *, #7594, .T. ) ;
#17644 = DIRECTION ( 'NONE',  ( -1.000000000000000000, 0.000000000000000000, -0.000000000000000000 ) ) ;
#17645 = DIRECTION ( 'NONE',  ( 0.000000000000000000, 0.000000000000000000, 1.000000000000000000 ) ) ;
#17646 = CARTESIAN_POINT ( 'NONE',  ( 5.000000000000002665, 40.72878876293147954, 78.00747250042462611 ) ) ;
#17647 = AXIS2_PLACEMENT_3D ( 'NONE', #7218, #3676, #13949 ) ;
#17648 = CIRCLE ( 'NONE', #18000, 5.000000000000000000 ) ;
#17649 = CARTESIAN_POINT ( 'NONE',  ( 0.000000000000000000, -90.32141448704669529, -19.96189084378313794 ) ) ;
#17650 = DIRECTION ( 'NONE',  ( -1.000000000000000000, -0.000000000000000000, -0.000000000000000000 ) ) ;
#17651 = ORIENTED_EDGE ( 'NONE', *, *, #13788, .T. ) ;
#17652 = LINE ( 'NONE', #12232, #18696 ) ;
#17653 = DIRECTION ( 'NONE',  ( 0.000000000000000000, 0.000000000000000000, -1.000000000000000000 ) ) ;
#17654 = DIRECTION ( 'NONE',  ( -0.8432271980573100567, 6.583178742725224615E-17, -0.5375573387615669718 ) ) ;
#17655 = ORIENTED_EDGE ( 'NONE', *, *, #4759, .T. ) ;
#17656 = CARTESIAN_POINT ( 'NONE',  ( 10.00000000000000000, -81.97107881582211064, 22.71412948308539370 ) ) ;
#17657 = ORIENTED_EDGE ( 'NONE', *, *, #13414, .T. ) ;
#17658 = CIRCLE ( 'NONE', #13775, 88.00000000000000000 ) ;
#17659 = DIRECTION ( 'NONE',  ( 1.000000000000000000, 0.000000000000000000, 0.000000000000000000 ) ) ;
#17660 = VERTEX_POINT ( 'NONE', #11592 ) ;
#17661 = EDGE_LOOP ( 'NONE', ( #10771, #3148, #337, #17708 ) ) ;
#17662 = EDGE_CURVE ( 'NONE', #11869, #5926, #16451, .T. ) ;
#17663 = ORIENTED_EDGE ( 'NONE', *, *, #4323, .T. ) ;
#17664 = DIRECTION ( 'NONE',  ( -1.000000000000000000, 0.000000000000000000, 0.000000000000000000 ) ) ;
#17665 = ORIENTED_EDGE ( 'NONE', *, *, #5685, .F. ) ;
#17666 = FACE_OUTER_BOUND ( 'NONE', #6982, .T. ) ;
#17667 = DIRECTION ( 'NONE',  ( 1.000000000000000000, -0.000000000000000000, -0.000000000000000000 ) ) ;
#17668 = CARTESIAN_POINT ( 'NONE',  ( -10.00000000000000000, 0.000000000000000000, 0.000000000000000000 ) ) ;
#17669 = CARTESIAN_POINT ( 'NONE',  ( 5.000000000000000000, -69.74988376404053270, 53.65588238863315240 ) ) ;
#17670 = ADVANCED_FACE ( 'NONE', ( #14800 ), #13454, .F. ) ;
#17671 = DIRECTION ( 'NONE',  ( 1.000000000000000000, 0.000000000000000000, 0.000000000000000000 ) ) ;
#17672 = CARTESIAN_POINT ( 'NONE',  ( 10.00000000000000000, -72.58367602204218372, 49.75550195834843237 ) ) ;
#17673 = CARTESIAN_POINT ( 'NONE',  ( 10.00000000000000888, 0.000000000000000000, 0.000000000000000000 ) ) ;
#17674 = VECTOR ( 'NONE', #11455, 1000.000000000000000 ) ;
#17675 = DIRECTION ( 'NONE',  ( -1.000000000000000000, 0.000000000000000000, 0.000000000000000000 ) ) ;
#17676 = CARTESIAN_POINT ( 'NONE',  ( 10.00000000000000000, 46.93287725819779155, 70.94007663282461351 ) ) ;
#17677 = CYLINDRICAL_SURFACE ( 'NONE', #2008, 44.99999999999998579 ) ;
#17678 = EDGE_LOOP ( 'NONE', ( #12570, #12474, #15339, #25 ) ) ;
#17679 = ORIENTED_EDGE ( 'NONE', *, *, #10165, .F. ) ;
#17680 = ORIENTED_EDGE ( 'NONE', *, *, #16896, .T. ) ;
#17681 = ORIENTED_EDGE ( 'NONE', *, *, #10816, .F. ) ;
#17682 = EDGE_CURVE ( 'NONE', #15531, #5375, #9048, .T. ) ;
#17683 = EDGE_CURVE ( 'NONE', #18295, #19585, #12225, .T. ) ;
#17684 = MECHANICAL_DESIGN_GEOMETRIC_PRESENTATION_REPRESENTATION (  '', ( #6414 ), #5679 ) ;
#17685 = ORIENTED_EDGE ( 'NONE', *, *, #15656, .F. ) ;
#17686 = CARTESIAN_POINT ( 'NONE',  ( 0.000000000000000000, 0.000000000000000000, 0.000000000000000000 ) ) ;
#17687 = EDGE_LOOP ( 'NONE', ( #15932, #19551, #20111, #19548 ) ) ;
#17688 = FACE_OUTER_BOUND ( 'NONE', #11186, .T. ) ;
#17689 = CARTESIAN_POINT ( 'NONE',  ( 0.000000000000000000, -56.34908017029516714, -63.71789861856507997 ) ) ;
#17690 = DIRECTION ( 'NONE',  ( -1.000000000000000000, -0.000000000000000000, -0.000000000000000000 ) ) ;
#17691 = LINE ( 'NONE', #21118, #19691 ) ;
#17692 = CARTESIAN_POINT ( 'NONE',  ( 10.00000000000000000, -77.39385041987173963, 35.28996114464576550 ) ) ;
#17693 = CARTESIAN_POINT ( 'NONE',  ( 10.00000000000000000, 0.000000000000000000, 0.000000000000000000 ) ) ;
#17694 = DIRECTION ( 'NONE',  ( -0.000000000000000000, -0.000000000000000000, 1.000000000000000000 ) ) ;
#17695 = EDGE_CURVE ( 'NONE', #16928, #11100, #16120, .T. ) ;
#17696 = CARTESIAN_POINT ( 'NONE',  ( 0.000000000000000000, 41.87002153499110335, 74.04114219178059386 ) ) ;
#17697 = PRODUCT_DEFINITION_FORMATION_WITH_SPECIFIED_SOURCE ( 'ANY', '', #11423, .NOT_KNOWN. ) ;
#17698 = ORIENTED_EDGE ( 'NONE', *, *, #19569, .T. ) ;
#17699 = EDGE_CURVE ( 'NONE', #769, #18882, #9751, .T. ) ;
#17700 = CARTESIAN_POINT ( 'NONE',  ( 1.399999999999998579, 0.000000000000000000, -5.000000000000000000 ) ) ;
#17701 = FACE_OUTER_BOUND ( 'NONE', #3700, .T. ) ;
#17702 = CARTESIAN_POINT ( 'NONE',  ( 0.000000000000000000, 81.83745710415318797, -32.35167097270070258 ) ) ;
#17703 = EDGE_CURVE ( 'NONE', #4590, #827, #3847, .T. ) ;
#17704 = VERTEX_POINT ( 'NONE', #15328 ) ;
#17705 = EDGE_CURVE ( 'NONE', #10994, #6894, #2348, .T. ) ;
#17706 = EDGE_CURVE ( 'NONE', #21543, #7099, #418, .T. ) ;
#17707 = DIRECTION ( 'NONE',  ( -1.000000000000000000, -0.000000000000000000, -0.000000000000000000 ) ) ;
#17708 = ORIENTED_EDGE ( 'NONE', *, *, #20801, .T. ) ;
#17709 = ORIENTED_EDGE ( 'NONE', *, *, #2421, .F. ) ;
#17710 = DIRECTION ( 'NONE',  ( 0.5991806890052243650, -1.789069944041725506E-17, 0.8006138282113447469 ) ) ;
#17711 = FACE_OUTER_BOUND ( 'NONE', #14911, .T. ) ;
#17712 = EDGE_CURVE ( 'NONE', #75, #1096, #4120, .T. ) ;
#17713 = ORIENTED_EDGE ( 'NONE', *, *, #20581, .T. ) ;
#17714 = ORIENTED_EDGE ( 'NONE', *, *, #20691, .T. ) ;
#17715 = CARTESIAN_POINT ( 'NONE',  ( 10.00000000000000000, -29.29369617358407041, -87.74003855418429509 ) ) ;
#17716 = DIRECTION ( 'NONE',  ( -1.000000000000000000, 0.000000000000000000, 0.000000000000000000 ) ) ;
#17717 = EDGE_CURVE ( 'NONE', #18616, #6321, #20534, .T. ) ;
#17718 = DIRECTION ( 'NONE',  ( -1.000000000000000000, -0.000000000000000000, 0.000000000000000000 ) ) ;
#17719 = LINE ( 'NONE', #19265, #13340 ) ;
#17720 = DIRECTION ( 'NONE',  ( 0.000000000000000000, 0.000000000000000000, -1.000000000000000000 ) ) ;
#17721 = FACE_OUTER_BOUND ( 'NONE', #8418, .T. ) ;
#17722 = DIRECTION ( 'NONE',  ( 0.000000000000000000, 0.8660254037844361541, 0.5000000000000041078 ) ) ;
#17723 = DIRECTION ( 'NONE',  ( -1.000000000000000000, 0.000000000000000000, 0.000000000000000000 ) ) ;
#17724 = EDGE_CURVE ( 'NONE', #4269, #923, #21060, .T. ) ;
#17725 = DIRECTION ( 'NONE',  ( -1.000000000000000000, 0.000000000000000000, -0.000000000000000000 ) ) ;
#17726 = AXIS2_PLACEMENT_3D ( 'NONE', #20593, #484, #7227 ) ;
#17727 = ORIENTED_EDGE ( 'NONE', *, *, #9320, .F. ) ;
#17728 = EDGE_CURVE ( 'NONE', #18476, #11575, #4137, .T. ) ;
#17729 = APPLICATION_CONTEXT ( 'automotive_design' ) ;
#17730 = LINE ( 'NONE', #21158, #20332 ) ;
#17731 = ORIENTED_EDGE ( 'NONE', *, *, #9867, .T. ) ;
#17732 = EDGE_CURVE ( 'NONE', #8340, #8524, #1664, .T. ) ;
#17733 = DIRECTION ( 'NONE',  ( 1.000000000000000000, 0.000000000000000000, 0.000000000000000000 ) ) ;
#17734 = VERTEX_POINT ( 'NONE', #5616 ) ;
#17735 = CARTESIAN_POINT ( 'NONE',  ( 10.00000000000000000, -8.134922360106683570, 84.67002113262478247 ) ) ;
#17736 = LINE ( 'NONE', #2586, #8808 ) ;
#17737 = EDGE_LOOP ( 'NONE', ( #17363, #6728, #16854, #12798 ) ) ;
#17738 =( LENGTH_UNIT ( ) NAMED_UNIT ( * ) SI_UNIT ( .MILLI., .METRE. ) );
#17739 = ORIENTED_EDGE ( 'NONE', *, *, #14179, .T. ) ;
#17740 = AXIS2_PLACEMENT_3D ( 'NONE', #20338, #8290, #15023 ) ;
#17741 = EDGE_CURVE ( 'NONE', #11543, #13950, #11896, .T. ) ;
#17742 = ORIENTED_EDGE ( 'NONE', *, *, #18425, .T. ) ;
#17743 = VERTEX_POINT ( 'NONE', #12124 ) ;
#17744 = DIRECTION ( 'NONE',  ( 1.000000000000000000, 0.000000000000000000, 0.000000000000000000 ) ) ;
#17745 = CARTESIAN_POINT ( 'NONE',  ( 10.00000000000000000, 0.000000000000000000, 0.000000000000000000 ) ) ;
#17746 = AXIS2_PLACEMENT_3D ( 'NONE', #6413, #16770, #18225 ) ;
#17747 = VERTEX_POINT ( 'NONE', #15767 ) ;
#17748 = DIRECTION ( 'NONE',  ( 0.000000000000000000, 0.000000000000000000, 1.000000000000000000 ) ) ;
#17749 = CARTESIAN_POINT ( 'NONE',  ( 10.00000000000000000, 61.33825423015685629, 69.23910433415966281 ) ) ;
#17750 = CARTESIAN_POINT ( 'NONE',  ( 10.00000000000000000, -7.409634587003275819, 27.19958299168154880 ) ) ;
#17751 = DIRECTION ( 'NONE',  ( 0.000000000000000000, 0.6946583704589935904, 0.7193398003386546335 ) ) ;
#17752 = CARTESIAN_POINT ( 'NONE',  ( 0.000000000000000000, 0.000000000000000000, 0.000000000000000000 ) ) ;
#17753 = AXIS2_PLACEMENT_3D ( 'NONE', #17689, #12708, #14483 ) ;
#17754 = ORIENTED_EDGE ( 'NONE', *, *, #1119, .T. ) ;
#17755 = EDGE_CURVE ( 'NONE', #7932, #10994, #18876, .T. ) ;
#17756 = DIRECTION ( 'NONE',  ( 0.000000000000000000, -0.7431448254773861395, -0.6691306063588671194 ) ) ;
#17757 = DIRECTION ( 'NONE',  ( 0.000000000000000000, 0.1391731009600657709, -0.9902680687415702510 ) ) ;
#17758 = AXIS2_PLACEMENT_3D ( 'NONE', #1813, #11755, #14854 ) ;
#17759 = EDGE_CURVE ( 'NONE', #13983, #18351, #5203, .T. ) ;
#17760 = CARTESIAN_POINT ( 'NONE',  ( -10.00000000000000000, 0.000000000000000000, 0.000000000000000000 ) ) ;
#17761 = EDGE_LOOP ( 'NONE', ( #8455, #10883, #1353, #10710 ) ) ;
#17762 = CARTESIAN_POINT ( 'NONE',  ( 5.000000000000002665, -46.07110168784872428, 74.97635353408365688 ) ) ;
#17763 = ORIENTED_EDGE ( 'NONE', *, *, #16652, .T. ) ;
#17764 = CARTESIAN_POINT ( 'NONE',  ( -1.500000000000000000, 15.00000000000000000, 7.000000000000000000 ) ) ;
#17765 = ORIENTED_EDGE ( 'NONE', *, *, #14563, .T. ) ;
#17766 = AXIS2_PLACEMENT_3D ( 'NONE', #9916, #3074, #19763 ) ;
#17767 = VERTEX_POINT ( 'NONE', #13681 ) ;
#17768 = ORIENTED_EDGE ( 'NONE', *, *, #5305, .T. ) ;
#17769 = DIRECTION ( 'NONE',  ( 0.000000000000000000, 1.000000000000000000, 0.000000000000000000 ) ) ;
#17770 = ORIENTED_EDGE ( 'NONE', *, *, #20890, .F. ) ;
#17771 = DIRECTION ( 'NONE',  ( 0.000000000000000000, 0.000000000000000000, 1.000000000000000000 ) ) ;
#17772 = CIRCLE ( 'NONE', #7186, 92.50100000000003320 ) ;
#17773 = DIRECTION ( 'NONE',  ( -1.000000000000000000, 0.000000000000000000, 0.000000000000000000 ) ) ;
#17774 = DIRECTION ( 'NONE',  ( 0.000000000000000000, 0.000000000000000000, 1.000000000000000000 ) ) ;
#17775 = DIRECTION ( 'NONE',  ( 1.000000000000000000, 0.000000000000000000, 0.000000000000000000 ) ) ;
#17776 = AXIS2_PLACEMENT_3D ( 'NONE', #8481, #3503, #3395 ) ;
#17777 = AXIS2_PLACEMENT_3D ( 'NONE', #9959, #20034, #3015 ) ;
#17778 = DIRECTION ( 'NONE',  ( 1.000000000000000000, 0.000000000000000000, 0.000000000000000000 ) ) ;
#17779 = CARTESIAN_POINT ( 'NONE',  ( 0.000000000000000000, 0.000000000000000000, 0.000000000000000000 ) ) ;
#17780 = ADVANCED_FACE ( 'NONE', ( #15445 ), #10354, .F. ) ;
#17781 = CARTESIAN_POINT ( 'NONE',  ( 5.000000000000000000, 87.92084725184948013, 3.731570516143270400 ) ) ;
#17782 = DIRECTION ( 'NONE',  ( 0.000000000000000000, 0.000000000000000000, -1.000000000000000000 ) ) ;
#17783 = AXIS2_PLACEMENT_3D ( 'NONE', #7910, #4599, #6712 ) ;
#17784 = DIRECTION ( 'NONE',  ( 1.000000000000000000, 0.000000000000000000, 0.000000000000000000 ) ) ;
#17785 = ORIENTED_EDGE ( 'NONE', *, *, #2034, .T. ) ;
#17786 = EDGE_LOOP ( 'NONE', ( #19073, #8937, #10615, #18125 ) ) ;
#17787 = CIRCLE ( 'NONE', #8267, 0.1000000000000002554 ) ;
#17788 = ORIENTED_EDGE ( 'NONE', *, *, #7235, .T. ) ;
#17789 = ORIENTED_EDGE ( 'NONE', *, *, #6217, .F. ) ;
#17790 = VERTEX_POINT ( 'NONE', #10254 ) ;
#17791 = CARTESIAN_POINT ( 'NONE',  ( 0.000000000000000000, 0.000000000000000000, 0.000000000000000000 ) ) ;
#17792 = CIRCLE ( 'NONE', #16012, 92.50100000000000477 ) ;
#17793 = ORIENTED_EDGE ( 'NONE', *, *, #6326, .T. ) ;
#17794 = DIRECTION ( 'NONE',  ( 0.000000000000000000, -0.4067366430758070917, 0.9135454576425978690 ) ) ;
#17795 = DIRECTION ( 'NONE',  ( 0.000000000000000000, 0.000000000000000000, 1.000000000000000000 ) ) ;
#17796 = CARTESIAN_POINT ( 'NONE',  ( 10.00000000000000000, 91.49386717542222414, 13.61276130277023810 ) ) ;
#17797 = AXIS2_PLACEMENT_3D ( 'NONE', #6152, #11110, #1166 ) ;
#17798 = DIRECTION ( 'NONE',  ( 0.000000000000000000, 0.000000000000000000, 1.000000000000000000 ) ) ;
#17799 = DIRECTION ( 'NONE',  ( 1.000000000000000000, 0.000000000000000000, 0.000000000000000000 ) ) ;
#17800 = DIRECTION ( 'NONE',  ( 1.000000000000000000, 0.000000000000000000, 0.000000000000000000 ) ) ;
#17801 = CIRCLE ( 'NONE', #20286, 7.500000000000000000 ) ;
#17802 = DIRECTION ( 'NONE',  ( 0.000000000000000000, 0.9510565162951544194, -0.3090169943749450643 ) ) ;
#17803 = DIRECTION ( 'NONE',  ( -1.000000000000000000, 0.000000000000000000, 0.000000000000000000 ) ) ;
#17804 = CARTESIAN_POINT ( 'NONE',  ( 5.000000000000000000, 31.88200538760793634, -2.745493118647104325 ) ) ;
#17805 = EDGE_CURVE ( 'NONE', #17876, #7364, #256, .T. ) ;
#17806 = VERTEX_POINT ( 'NONE', #2286 ) ;
#17807 = DIRECTION ( 'NONE',  ( -1.000000000000000000, -0.000000000000000000, -0.000000000000000000 ) ) ;
#17808 = AXIS2_PLACEMENT_3D ( 'NONE', #15467, #2310, #6976 ) ;
#17809 = AXIS2_PLACEMENT_3D ( 'NONE', #19124, #9063, #3883 ) ;
#17810 = ORIENTED_EDGE ( 'NONE', *, *, #3159, .T. ) ;
#17811 = ADVANCED_FACE ( 'NONE', ( #9021 ), #12024, .F. ) ;
#17812 = VECTOR ( 'NONE', #13225, 1000.000000000000000 ) ;
#17813 = DIRECTION ( 'NONE',  ( 0.000000000000000000, -0.06975647374411146628, -0.9975640502598251969 ) ) ;
#17814 = CARTESIAN_POINT ( 'NONE',  ( 1.129531546211711479, 0.000000000000000000, -5.612499999999999822 ) ) ;
#17815 = ORIENTED_EDGE ( 'NONE', *, *, #16665, .T. ) ;
#17816 = CYLINDRICAL_SURFACE ( 'NONE', #16539, 44.99999999999999289 ) ;
#17817 = EDGE_LOOP ( 'NONE', ( #19133, #1757, #2296, #2759, #13316, #9116 ) ) ;
#17818 = ORIENTED_EDGE ( 'NONE', *, *, #18018, .T. ) ;
#17819 = CIRCLE ( 'NONE', #9335, 27.49900000000000944 ) ;
#17820 = DIRECTION ( 'NONE',  ( 0.9407010676598062116, -8.106418413306812255E-17, 0.3392366449894539948 ) ) ;
#17821 = EDGE_CURVE ( 'NONE', #3424, #12605, #20373, .T. ) ;
#17822 = DIRECTION ( 'NONE',  ( -1.000000000000000000, -0.000000000000000000, -0.000000000000000000 ) ) ;
#17823 = ORIENTED_EDGE ( 'NONE', *, *, #7461, .F. ) ;
#17824 = ORIENTED_EDGE ( 'NONE', *, *, #14156, .F. ) ;
#17825 = DIRECTION ( 'NONE',  ( 1.000000000000000000, 0.000000000000000000, 0.000000000000000000 ) ) ;
#17826 = DIRECTION ( 'NONE',  ( -1.000000000000000000, 0.000000000000000000, 0.000000000000000000 ) ) ;
#17827 = DIRECTION ( 'NONE',  ( -1.000000000000000000, -0.000000000000000000, -0.000000000000000000 ) ) ;
#17828 = CARTESIAN_POINT ( 'NONE',  ( 0.000000000000000000, -65.64563793391867819, 54.09103124042793098 ) ) ;
#17829 = AXIS2_PLACEMENT_3D ( 'NONE', #12440, #9229, #741 ) ;
#17830 = DIRECTION ( 'NONE',  ( 0.000000000000000000, -0.9510565162951565288, 0.3090169943749382919 ) ) ;
#17831 = FACE_OUTER_BOUND ( 'NONE', #17552, .T. ) ;
#17832 = CIRCLE ( 'NONE', #1600, 0.1000000000000002554 ) ;
#17833 = DIRECTION ( 'NONE',  ( 0.000000000000000000, -1.000000000000000000, 0.000000000000000000 ) ) ;
#17834 = DIRECTION ( 'NONE',  ( 0.000000000000000000, 0.000000000000000000, 1.000000000000000000 ) ) ;
#17836 = VECTOR ( 'NONE', #3561, 1000.000000000000000 ) ;
#17835 = CARTESIAN_POINT ( 'NONE',  ( 10.00000000000000000, 33.95793648385932784, -86.04239391577952745 ) ) ;
#17837 = EDGE_CURVE ( 'NONE', #17412, #15910, #7593, .T. ) ;
#17838 = EDGE_CURVE ( 'NONE', #12967, #5617, #8366, .T. ) ;
#17839 = ADVANCED_FACE ( 'NONE', ( #21183, #9133 ), #6164, .T. ) ;
#17840 = EDGE_LOOP ( 'NONE', ( #13927, #15144, #17360, #1858 ) ) ;
#17841 = CARTESIAN_POINT ( 'NONE',  ( 10.00000000000000000, 28.00896854771991329, 15.47571261340933368 ) ) ;
#17842 = EDGE_CURVE ( 'NONE', #3530, #3300, #17875, .T. ) ;
#17843 = EDGE_LOOP ( 'NONE', ( #6193, #20785, #1910, #18771 ) ) ;
#17844 = DIRECTION ( 'NONE',  ( -1.000000000000000000, 0.000000000000000000, 0.000000000000000000 ) ) ;
#17845 = CARTESIAN_POINT ( 'NONE',  ( 0.000000000000000000, -9.366510754379408610, 25.85466064925422458 ) ) ;
#17846 = AXIS2_PLACEMENT_3D ( 'NONE', #11174, #1118, #7763 ) ;
#17847 = FACE_OUTER_BOUND ( 'NONE', #12329, .T. ) ;
#17848 = AXIS2_PLACEMENT_3D ( 'NONE', #20698, #373, #7220 ) ;
#17849 = VERTEX_POINT ( 'NONE', #2506 ) ;
#17850 = CIRCLE ( 'NONE', #1614, 27.49900000000000588 ) ;
#17851 = EDGE_CURVE ( 'NONE', #17170, #6729, #6267, .T. ) ;
#17852 = AXIS2_PLACEMENT_3D ( 'NONE', #10838, #17590, #2450 ) ;
#17853 = ORIENTED_EDGE ( 'NONE', *, *, #17025, .F. ) ;
#17854 = ORIENTED_EDGE ( 'NONE', *, *, #20341, .T. ) ;
#17855 = ORIENTED_EDGE ( 'NONE', *, *, #16389, .F. ) ;
#17856 = DIRECTION ( 'NONE',  ( 0.000000000000000000, 0.000000000000000000, 1.000000000000000000 ) ) ;
#17857 = CARTESIAN_POINT ( 'NONE',  ( 10.00000000000000000, 92.49798535263880694, -0.7467976319023919007 ) ) ;
#17858 = ORIENTED_EDGE ( 'NONE', *, *, #15795, .T. ) ;
#17859 = EDGE_CURVE ( 'NONE', #1594, #19677, #12594, .T. ) ;
#17860 = FACE_OUTER_BOUND ( 'NONE', #3243, .T. ) ;
#17861 = CARTESIAN_POINT ( 'NONE',  ( 10.00000000000000000, -5.479102470009884485, -87.82926298292120748 ) ) ;
#17862 = DIRECTION ( 'NONE',  ( -1.000000000000000000, -0.000000000000000000, -0.000000000000000000 ) ) ;
#17863 = DIRECTION ( 'NONE',  ( 0.000000000000000000, 0.000000000000000000, 1.000000000000000000 ) ) ;
#17864 = AXIS2_PLACEMENT_3D ( 'NONE', #9963, #6783, #14943 ) ;
#17865 = CARTESIAN_POINT ( 'NONE',  ( 10.00000000000000000, 0.000000000000000000, 0.000000000000000000 ) ) ;
#17866 = APPLICATION_CONTEXT ( 'automotive_design' ) ;
#17867 = CIRCLE ( 'NONE', #10797, 6.887500000000022382 ) ;
#17868 = ORIENTED_EDGE ( 'NONE', *, *, #19630, .T. ) ;
#17869 = STYLED_ITEM ( 'NONE', ( #18385 ), #13088 ) ;
#17870 = DIRECTION ( 'NONE',  ( -1.000000000000000000, 0.000000000000000000, 0.000000000000000000 ) ) ;
#17871 = AXIS2_PLACEMENT_3D ( 'NONE', #643, #2187, #6064 ) ;
#17872 = EDGE_CURVE ( 'NONE', #923, #13383, #15771, .T. ) ;
#17873 = DIRECTION ( 'NONE',  ( 0.000000000000000000, 0.000000000000000000, -1.000000000000000000 ) ) ;
#17874 = VERTEX_POINT ( 'NONE', #1071 ) ;
#17875 = LINE ( 'NONE', #4384, #4851 ) ;
#17876 = VERTEX_POINT ( 'NONE', #2399 ) ;
#17877 = CARTESIAN_POINT ( 'NONE',  ( 0.000000000000000000, 0.000000000000000000, 3.000000000000000000 ) ) ;
#17878 = DIRECTION ( 'NONE',  ( -1.000000000000000000, -0.000000000000000000, -0.000000000000000000 ) ) ;
#17879 = ORIENTED_EDGE ( 'NONE', *, *, #20228, .T. ) ;
#17880 = FACE_OUTER_BOUND ( 'NONE', #9373, .T. ) ;
#17881 = ADVANCED_FACE ( 'NONE', ( #1177 ), #17988, .F. ) ;
#17882 = ORIENTED_EDGE ( 'NONE', *, *, #14682, .T. ) ;
#17883 = ORIENTED_EDGE ( 'NONE', *, *, #5024, .T. ) ;
#17884 = ORIENTED_EDGE ( 'NONE', *, *, #4434, .T. ) ;
#17885 = DIRECTION ( 'NONE',  ( 0.000000000000000000, 0.000000000000000000, 1.000000000000000000 ) ) ;
#17886 = EDGE_CURVE ( 'NONE', #8737, #4066, #15424, .T. ) ;
#17887 = CIRCLE ( 'NONE', #10109, 9.999999999999998224 ) ;
#17888 = VERTEX_POINT ( 'NONE', #19635 ) ;
#17889 = DIRECTION ( 'NONE',  ( 0.000000000000000000, 0.000000000000000000, 1.000000000000000000 ) ) ;
#17890 = CARTESIAN_POINT ( 'NONE',  ( 10.00000000000000000, -83.35585896458628952, 16.94078559807922346 ) ) ;
#17891 = CARTESIAN_POINT ( 'NONE',  ( 10.00000000000000000, -12.46320060045743361, 29.47318494484024143 ) ) ;
#17892 = ADVANCED_FACE ( 'NONE', ( #9231 ), #4498, .T. ) ;
#17893 = CARTESIAN_POINT ( 'NONE',  ( 10.00000000000000000, -91.49386717542229519, 13.61276130276963414 ) ) ;
#17894 = ADVANCED_FACE ( 'NONE', ( #12666 ), #15979, .T. ) ;
#17895 = CARTESIAN_POINT ( 'NONE',  ( 10.00000000000000000, 0.000000000000000000, 0.000000000000000000 ) ) ;
#17896 = CYLINDRICAL_SURFACE ( 'NONE', #4678, 27.49900000000000233 ) ;
#17897 = CARTESIAN_POINT ( 'NONE',  ( 5.000000000000002665, 12.90135963484081216, 87.04915231966650424 ) ) ;
#17898 = CARTESIAN_POINT ( 'NONE',  ( 10.00000000000000000, -1.959304526717989381, 27.42911093658674204 ) ) ;
#17899 = AXIS2_PLACEMENT_3D ( 'NONE', #10274, #20345, #2104 ) ;
#17900 = AXIS2_PLACEMENT_3D ( 'NONE', #12348, #14113, #16997 ) ;
#17901 = AXIS2_PLACEMENT_3D ( 'NONE', #14129, #10809, #17563 ) ;
#17902 = DIRECTION ( 'NONE',  ( -1.000000000000000000, 0.000000000000000000, 0.000000000000000000 ) ) ;
#17903 = VERTEX_POINT ( 'NONE', #2612 ) ;
#17904 = VERTEX_POINT ( 'NONE', #16308 ) ;
#17905 = EDGE_LOOP ( 'NONE', ( #5430, #21754, #12636, #15802 ) ) ;
#17906 = EDGE_LOOP ( 'NONE', ( #9643, #5526, #13078, #18311 ) ) ;
#17907 = ORIENTED_EDGE ( 'NONE', *, *, #11209, .T. ) ;
#17908 = DIRECTION ( 'NONE',  ( -1.000000000000000000, -0.000000000000000000, -0.000000000000000000 ) ) ;
#17909 = CIRCLE ( 'NONE', #8738, 88.00000000000000000 ) ;
#17910 = ORIENTED_EDGE ( 'NONE', *, *, #7337, .F. ) ;
#17911 = DIRECTION ( 'NONE',  ( 1.000000000000000000, 0.000000000000000000, 0.000000000000000000 ) ) ;
#17912 = AXIS2_PLACEMENT_3D ( 'NONE', #5266, #12320, #8884 ) ;
#17913 = CIRCLE ( 'NONE', #12964, 27.49900000000000233 ) ;
#17914 = CYLINDRICAL_SURFACE ( 'NONE', #85, 44.99999999999999289 ) ;
#17915 = VECTOR ( 'NONE', #9336, 1000.000000000000000 ) ;
#17916 = CARTESIAN_POINT ( 'NONE',  ( 1.399999999999998579, 0.000000000000000000, -7.500000000000021316 ) ) ;
#17917 = DIRECTION ( 'NONE',  ( -1.000000000000000000, 0.000000000000000000, -0.000000000000000000 ) ) ;
#17918 = DIRECTION ( 'NONE',  ( 0.000000000000000000, 0.8660254037844398178, -0.4999999999999979461 ) ) ;
#17919 = CARTESIAN_POINT ( 'NONE',  ( 0.000000000000000000, 84.12297548659721258, 32.40974838672968872 ) ) ;
#17920 = CARTESIAN_POINT ( 'NONE',  ( 10.00000000000000000, -84.12297548659712731, -12.59025161327086906 ) ) ;
#17921 = CARTESIAN_POINT ( 'NONE',  ( 10.00000000000000000, -51.10509369859486384, 77.10190917907182495 ) ) ;
#17922 = ORIENTED_EDGE ( 'NONE', *, *, #15653, .F. ) ;
#17923 = DIRECTION ( 'NONE',  ( 0.000000000000000000, 0.3420201433256630508, 0.9396926207859104263 ) ) ;
#17924 = CIRCLE ( 'NONE', #20745, 92.50100000000000477 ) ;
#17925 = AXIS2_PLACEMENT_3D ( 'NONE', #14202, #20949, #21059 ) ;
#17926 = ORIENTED_EDGE ( 'NONE', *, *, #5940, .T. ) ;
#17927 = CARTESIAN_POINT ( 'NONE',  ( 1.400000000000000133, 6.245698675651501825E-16, 5.100000000000000533 ) ) ;
#17928 = CARTESIAN_POINT ( 'NONE',  ( 0.000000000000000000, -70.37753541435900217, -60.02863908169706519 ) ) ;
#17929 = ORIENTED_EDGE ( 'NONE', *, *, #15652, .T. ) ;
#17930 = DIRECTION ( 'NONE',  ( -1.000000000000000000, 0.000000000000000000, -0.000000000000000000 ) ) ;
#17931 = EDGE_LOOP ( 'NONE', ( #15659, #5071, #8814, #14888 ) ) ;
#17932 = VERTEX_POINT ( 'NONE', #19191 ) ;
#17933 = DIRECTION ( 'NONE',  ( 1.000000000000000000, 0.000000000000000000, 0.000000000000000000 ) ) ;
#17934 = AXIS2_PLACEMENT_3D ( 'NONE', #17040, #136, #1689 ) ;
#17935 = CARTESIAN_POINT ( 'NONE',  ( 5.000000000000000000, 61.60362715319122628, -62.84101464466179721 ) ) ;
#17936 = ORIENTED_EDGE ( 'NONE', *, *, #2313, .T. ) ;
#17937 = EDGE_CURVE ( 'NONE', #19614, #4068, #12238, .T. ) ;
#17938 = VERTEX_POINT ( 'NONE', #7703 ) ;
#17939 = CARTESIAN_POINT ( 'NONE',  ( 5.000000000000000000, -51.18896083639317851, 71.57995730992162464 ) ) ;
#17940 = CARTESIAN_POINT ( 'NONE',  ( 10.00000000000000000, 24.73395913766463750, 12.01774797440586084 ) ) ;
#17941 = CIRCLE ( 'NONE', #8765, 88.00000000000000000 ) ;
#17942 = DIRECTION ( 'NONE',  ( -1.000000000000000000, -0.000000000000000000, -0.000000000000000000 ) ) ;
#17943 = CARTESIAN_POINT ( 'NONE',  ( 0.000000000000000000, 11.59241532900744787, -87.23311244498727035 ) ) ;
#17944 = CIRCLE ( 'NONE', #2781, 27.49900000000000233 ) ;
#17945 =( NAMED_UNIT ( * ) SI_UNIT ( $, .STERADIAN. ) SOLID_ANGLE_UNIT ( ) );
#17946 = AXIS2_PLACEMENT_3D ( 'NONE', #20136, #18264, #3114 ) ;
#17947 = DIRECTION ( 'NONE',  ( 0.000000000000000000, 0.2756373558169932791, 0.9612616959383205595 ) ) ;
#17948 = VECTOR ( 'NONE', #13370, 1000.000000000000000 ) ;
#17949 = EDGE_CURVE ( 'NONE', #12094, #15608, #6630, .T. ) ;
#17950 = DIRECTION ( 'NONE',  ( 1.000000000000000000, 0.000000000000000000, 0.000000000000000000 ) ) ;
#17951 = DIRECTION ( 'NONE',  ( -1.000000000000000000, 0.000000000000000000, 0.000000000000000000 ) ) ;
#17952 = CARTESIAN_POINT ( 'NONE',  ( 10.00000000000000000, -72.53479564998815476, 44.42851404693331574 ) ) ;
#17953 = ORIENTED_EDGE ( 'NONE', *, *, #17582, .F. ) ;
#17954 = DIRECTION ( 'NONE',  ( 0.000000000000000000, 0.000000000000000000, 1.000000000000000000 ) ) ;
#17955 = VERTEX_POINT ( 'NONE', #17544 ) ;
#17956 = CYLINDRICAL_SURFACE ( 'NONE', #3820, 44.99999999999998579 ) ;
#17957 = AXIS2_PLACEMENT_3D ( 'NONE', #8923, #15563, #8503 ) ;
#17958 = SURFACE_STYLE_USAGE ( .BOTH. , #12640 ) ;
#17959 = CIRCLE ( 'NONE', #21848, 27.49900000000000233 ) ;
#17960 = CIRCLE ( 'NONE', #4915, 115.1000000000000227 ) ;
#17961 = CARTESIAN_POINT ( 'NONE',  ( 0.000000000000000000, 0.000000000000000000, 0.000000000000000000 ) ) ;
#17962 = VECTOR ( 'NONE', #554, 1000.000000000000000 ) ;
#17963 = ORIENTED_EDGE ( 'NONE', *, *, #3559, .F. ) ;
#17964 = SURFACE_STYLE_USAGE ( .BOTH. , #1053 ) ;
#17965 = VERTEX_POINT ( 'NONE', #5834 ) ;
#17966 = ORIENTED_EDGE ( 'NONE', *, *, #16491, .F. ) ;
#17967 = EDGE_CURVE ( 'NONE', #2155, #15044, #18604, .T. ) ;
#17968 = ADVANCED_FACE ( 'NONE', ( #6720 ), #18085, .F. ) ;
#17969 = ORIENTED_EDGE ( 'NONE', *, *, #12289, .T. ) ;
#17970 = ADVANCED_FACE ( 'NONE', ( #16643 ), #21402, .F. ) ;
#17971 = DIRECTION ( 'NONE',  ( 1.000000000000000000, 0.000000000000000000, 0.000000000000000000 ) ) ;
#17972 = DIRECTION ( 'NONE',  ( -1.000000000000000000, -0.000000000000000000, -0.000000000000000000 ) ) ;
#17973 = VERTEX_POINT ( 'NONE', #14656 ) ;
#17974 = ADVANCED_FACE ( 'NONE', ( #12999 ), #1409, .F. ) ;
#17975 = CARTESIAN_POINT ( 'NONE',  ( 0.000000000000000000, -81.32027326007897727, 44.08455690949027428 ) ) ;
#17976 = LINE ( 'NONE', #9547, #5941 ) ;
#17977 = DIRECTION ( 'NONE',  ( 0.000000000000000000, 0.000000000000000000, 1.000000000000000000 ) ) ;
#17978 = CARTESIAN_POINT ( 'NONE',  ( 0.000000000000000000, 86.54587337002898551, -15.93147207946920396 ) ) ;
#17979 = LINE ( 'NONE', #16086, #9079 ) ;
#17980 = VECTOR ( 'NONE', #3605, 1000.000000000000000 ) ;
#17981 = ORIENTED_EDGE ( 'NONE', *, *, #1275, .T. ) ;
#17982 = CIRCLE ( 'NONE', #5628, 27.49900000000000233 ) ;
#17983 = CARTESIAN_POINT ( 'NONE',  ( 10.00000000000000000, -52.96496548042809138, -66.55750800669412115 ) ) ;
#17984 = ADVANCED_FACE ( 'NONE', ( #21611 ), #4709, .T. ) ;
#17985 = DIRECTION ( 'NONE',  ( 0.000000000000000000, 0.000000000000000000, 1.000000000000000000 ) ) ;
#17986 = ORIENTED_EDGE ( 'NONE', *, *, #2299, .T. ) ;
#17987 = ADVANCED_FACE ( 'NONE', ( #4608 ), #11448, .F. ) ;
#17988 = CYLINDRICAL_SURFACE ( 'NONE', #10829, 44.99999999999999289 ) ;
#17989 = ORIENTED_EDGE ( 'NONE', *, *, #12409, .T. ) ;
#17990 = PLANE ( 'NONE',  #6331 ) ;
#17991 = CARTESIAN_POINT ( 'NONE',  ( 10.00000000000000000, 0.000000000000000000, 0.000000000000000000 ) ) ;
#17992 = ORIENTED_EDGE ( 'NONE', *, *, #7826, .T. ) ;
#17993 = PLANE ( 'NONE',  #2145 ) ;
#17994 = AXIS2_PLACEMENT_3D ( 'NONE', #9622, #17716, #19807 ) ;
#17995 = VERTEX_POINT ( 'NONE', #18204 ) ;
#17996 = EDGE_LOOP ( 'NONE', ( #19815, #4825, #8605, #7714 ) ) ;
#17997 = EDGE_CURVE ( 'NONE', #8941, #18330, #16542, .T. ) ;
#17998 = VECTOR ( 'NONE', #43, 1000.000000000000000 ) ;
#17999 = FACE_OUTER_BOUND ( 'NONE', #18572, .T. ) ;
#18000 = AXIS2_PLACEMENT_3D ( 'NONE', #13761, #21827, #20176 ) ;
#18001 = ORIENTED_EDGE ( 'NONE', *, *, #16622, .T. ) ;
#18002 = DIRECTION ( 'NONE',  ( 0.000000000000000000, 0.000000000000000000, 1.000000000000000000 ) ) ;
#18003 = ADVANCED_FACE ( 'NONE', ( #8247 ), #10113, .F. ) ;
#18004 = DIRECTION ( 'NONE',  ( 0.000000000000000000, -8.943463253924873884E-15, -1.000000000000000000 ) ) ;
#18005 = CARTESIAN_POINT ( 'NONE',  ( 10.00000000000000000, -86.77540292929691645, -14.62974526292806843 ) ) ;
#18006 = DIRECTION ( 'NONE',  ( 0.000000000000000000, -0.3420201433256569445, -0.9396926207859125357 ) ) ;
#18007 = CARTESIAN_POINT ( 'NONE',  ( 10.00000000000000000, -7.240962358591787940, 31.16999300804311801 ) ) ;
#18008 = CARTESIAN_POINT ( 'NONE',  ( 5.000000000000000000, 56.05743251323954013, -67.83483072893743326 ) ) ;
#18009 = CARTESIAN_POINT ( 'NONE',  ( 10.00000000000000000, -39.87723064937059547, -83.46401306393613595 ) ) ;
#18010 = CARTESIAN_POINT ( 'NONE',  ( -10.00000000000000000, 0.000000000000000000, 0.000000000000000000 ) ) ;
#18011 = EDGE_CURVE ( 'NONE', #16010, #6503, #10486, .T. ) ;
#18012 = AXIS2_PLACEMENT_3D ( 'NONE', #10737, #20806, #15719 ) ;
#18013 = EDGE_CURVE ( 'NONE', #289, #19331, #9665, .T. ) ;
#18014 = FACE_OUTER_BOUND ( 'NONE', #1540, .T. ) ;
#18015 = ORIENTED_EDGE ( 'NONE', *, *, #3118, .F. ) ;
#18016 = VERTEX_POINT ( 'NONE', #14876 ) ;
#18017 = ADVANCED_FACE ( 'NONE', ( #13320 ), #19961, .T. ) ;
#18018 = EDGE_CURVE ( 'NONE', #16375, #4982, #13310, .T. ) ;
#18019 = VERTEX_POINT ( 'NONE', #20182 ) ;
#18020 = ORIENTED_EDGE ( 'NONE', *, *, #2317, .F. ) ;
#18021 = ORIENTED_EDGE ( 'NONE', *, *, #14630, .F. ) ;
#18022 = FACE_OUTER_BOUND ( 'NONE', #18559, .T. ) ;
#18023 = EDGE_CURVE ( 'NONE', #9734, #19710, #8036, .T. ) ;
#18024 = ORIENTED_EDGE ( 'NONE', *, *, #9290, .F. ) ;
#18025 = CARTESIAN_POINT ( 'NONE',  ( 0.000000000000000000, 0.000000000000000000, 0.000000000000000000 ) ) ;
#18026 = AXIS2_PLACEMENT_3D ( 'NONE', #7096, #11952, #8846 ) ;
#18027 = CARTESIAN_POINT ( 'NONE',  ( -8.900000000000019895, 0.000000000000000000, 0.000000000000000000 ) ) ;
#18028 = DIRECTION ( 'NONE',  ( 0.000000000000000000, 0.000000000000000000, 1.000000000000000000 ) ) ;
#18029 = DIRECTION ( 'NONE',  ( 1.000000000000000000, 0.000000000000000000, 0.000000000000000000 ) ) ;
#18030 = LINE ( 'NONE', #14698, #21043 ) ;
#18031 = CARTESIAN_POINT ( 'NONE',  ( 0.000000000000000000, -83.35585896458628952, 16.94078559807922346 ) ) ;
#18032 = CARTESIAN_POINT ( 'NONE',  ( 10.00000000000000000, 0.000000000000000000, 0.000000000000000000 ) ) ;
#18033 = ORIENTED_EDGE ( 'NONE', *, *, #9183, .T. ) ;
#18034 = CARTESIAN_POINT ( 'NONE',  ( 0.000000000000000000, 0.000000000000000000, 0.000000000000000000 ) ) ;
#18035 = AXIS2_PLACEMENT_3D ( 'NONE', #9906, #8362, #11684 ) ;
#18036 = ORIENTED_EDGE ( 'NONE', *, *, #8428, .F. ) ;
#18037 = EDGE_CURVE ( 'NONE', #14060, #15149, #18524, .T. ) ;
#18038 = DIRECTION ( 'NONE',  ( -1.000000000000000000, -0.000000000000000000, 0.000000000000000000 ) ) ;
#18039 = CARTESIAN_POINT ( 'NONE',  ( 0.000000000000000000, 21.31452625070926743, 82.34610137166127686 ) ) ;
#18040 = ORIENTED_EDGE ( 'NONE', *, *, #8274, .F. ) ;
#18041 = DIRECTION ( 'NONE',  ( 0.000000000000000000, -0.4067366430758070361, 0.9135454576425978690 ) ) ;
#18042 = ORIENTED_EDGE ( 'NONE', *, *, #182, .F. ) ;
#18043 = VERTEX_POINT ( 'NONE', #9899 ) ;
#18044 = APPLICATION_PROTOCOL_DEFINITION ( 'draft international standard', 'automotive_design', 1998, #13334 ) ;
#18045 = DIRECTION ( 'NONE',  ( -0.000000000000000000, -0.000000000000000000, 1.000000000000000000 ) ) ;
#18046 = ORIENTED_EDGE ( 'NONE', *, *, #549, .T. ) ;
#18047 = ORIENTED_EDGE ( 'NONE', *, *, #14737, .T. ) ;
#18048 = DIRECTION ( 'NONE',  ( 1.000000000000000000, 0.000000000000000000, 0.000000000000000000 ) ) ;
#18049 = FACE_OUTER_BOUND ( 'NONE', #19365, .T. ) ;
#18050 = CARTESIAN_POINT ( 'NONE',  ( 10.00000000000000000, 0.000000000000000000, 0.000000000000000000 ) ) ;
#18051 = DIRECTION ( 'NONE',  ( 0.000000000000000000, 0.000000000000000000, 1.000000000000000000 ) ) ;
#18052 = DIRECTION ( 'NONE',  ( 1.000000000000000000, 0.000000000000000000, 0.000000000000000000 ) ) ;
#18053 = AXIS2_PLACEMENT_3D ( 'NONE', #5273, #73, #10235 ) ;
#18054 = DIRECTION ( 'NONE',  ( -1.000000000000000000, -0.000000000000000000, -0.000000000000000000 ) ) ;
#18055 = CARTESIAN_POINT ( 'NONE',  ( 10.00000000000000000, -66.01871308925419157, -64.79170103523090063 ) ) ;
#18056 = CARTESIAN_POINT ( 'NONE',  ( 0.000000000000000000, 0.000000000000000000, 0.000000000000000000 ) ) ;
#18057 = CARTESIAN_POINT ( 'NONE',  ( 10.00000000000000000, 0.000000000000000000, 0.000000000000000000 ) ) ;
#18058 = ORIENTED_EDGE ( 'NONE', *, *, #8413, .T. ) ;
#18059 = EDGE_CURVE ( 'NONE', #13595, #10604, #5921, .T. ) ;
#18060 = ORIENTED_EDGE ( 'NONE', *, *, #21351, .T. ) ;
#18061 = FACE_OUTER_BOUND ( 'NONE', #20873, .T. ) ;
#18062 = VECTOR ( 'NONE', #19084, 1000.000000000000000 ) ;
#18063 = CARTESIAN_POINT ( 'NONE',  ( 5.000000000000000000, 75.87763420127832603, 44.57111876559750385 ) ) ;
#18064 = ORIENTED_EDGE ( 'NONE', *, *, #15837, .F. ) ;
#18065 = VERTEX_POINT ( 'NONE', #11679 ) ;
#18066 = ORIENTED_EDGE ( 'NONE', *, *, #5847, .T. ) ;
#18067 = ORIENTED_EDGE ( 'NONE', *, *, #10180, .T. ) ;
#18068 = CARTESIAN_POINT ( 'NONE',  ( 10.00000000000000000, 15.25521607131206459, 23.70650506194175478 ) ) ;
#18069 = FACE_OUTER_BOUND ( 'NONE', #11030, .T. ) ;
#18070 = ORIENTED_EDGE ( 'NONE', *, *, #3893, .F. ) ;
#18071 = CIRCLE ( 'NONE', #20882, 104.9000000000000341 ) ;
#18072 = CARTESIAN_POINT ( 'NONE',  ( 0.000000000000000000, 12.90135963484197212, -87.04915231966633371 ) ) ;
#18073 = CARTESIAN_POINT ( 'NONE',  ( 0.000000000000000000, 87.92084725184953697, -3.731570516142035387 ) ) ;
#18074 = LINE ( 'NONE', #14865, #2306 ) ;
#18075 = DIRECTION ( 'NONE',  ( 1.000000000000000000, 0.000000000000000000, 0.000000000000000000 ) ) ;
#18076 = DIRECTION ( 'NONE',  ( 1.000000000000000000, 0.000000000000000000, 0.000000000000000000 ) ) ;
#18077 = CARTESIAN_POINT ( 'NONE',  ( -7.395799999999999486, 0.000000000000000000, -114.9007999999999896 ) ) ;
#18078 = UNCERTAINTY_MEASURE_WITH_UNIT (LENGTH_MEASURE( 1.000000000000000082E-05 ), #18440, 'distance_accuracy_value', 'NONE');
#18079 = ORIENTED_EDGE ( 'NONE', *, *, #21240, .F. ) ;
#18080 = FACE_BOUND ( 'NONE', #7339, .T. ) ;
#18081 = AXIS2_PLACEMENT_3D ( 'NONE', #20787, #5655, #20887 ) ;
#18082 = DIRECTION ( 'NONE',  ( 0.000000000000000000, 0.000000000000000000, 1.000000000000000000 ) ) ;
#18083 = ADVANCED_FACE ( 'NONE', ( #18423 ), #5214, .T. ) ;
#18084 = ORIENTED_EDGE ( 'NONE', *, *, #13518, .F. ) ;
#18085 = CYLINDRICAL_SURFACE ( 'NONE', #9771, 88.00000000000000000 ) ;
#18086 = ORIENTED_EDGE ( 'NONE', *, *, #452, .F. ) ;
#18087 = AXIS2_PLACEMENT_3D ( 'NONE', #10266, #16677, #10043 ) ;
#18088 = FACE_BOUND ( 'NONE', #17471, .T. ) ;
#18089 = FACE_OUTER_BOUND ( 'NONE', #3413, .T. ) ;
#18090 = ORIENTED_EDGE ( 'NONE', *, *, #17618, .F. ) ;
#18091 = EDGE_CURVE ( 'NONE', #15149, #6824, #13679, .T. ) ;
#18092 = CARTESIAN_POINT ( 'NONE',  ( -90.00000000000000000, 0.000000000000000000, -104.9000000000000341 ) ) ;
#18093 = VERTEX_POINT ( 'NONE', #11996 ) ;
#18094 = ORIENTED_EDGE ( 'NONE', *, *, #3532, .F. ) ;
#18095 = CARTESIAN_POINT ( 'NONE',  ( 0.000000000000000000, 70.37753541435941429, 60.02863908169658202 ) ) ;
#18096 = ORIENTED_EDGE ( 'NONE', *, *, #17011, .T. ) ;
#18097 = EDGE_CURVE ( 'NONE', #15334, #4606, #11199, .T. ) ;
#18098 = LINE ( 'NONE', #16320, #3507 ) ;
#18099 = VECTOR ( 'NONE', #9038, 1000.000000000000000 ) ;
#18100 = DIRECTION ( 'NONE',  ( 1.000000000000000000, 0.000000000000000000, 0.000000000000000000 ) ) ;
#18101 = CYLINDRICAL_SURFACE ( 'NONE', #5063, 44.99999999999999289 ) ;
#18102 = CARTESIAN_POINT ( 'NONE',  ( 10.00000000000000000, -28.15804365424196121, 10.64184787299373269 ) ) ;
#18103 = AXIS2_PLACEMENT_3D ( 'NONE', #21765, #16579, #4978 ) ;
#18104 = CYLINDRICAL_SURFACE ( 'NONE', #18282, 44.99999999999999289 ) ;
#18105 = CARTESIAN_POINT ( 'NONE',  ( 0.000000000000000000, -24.17932380791704716, -20.96092317127029503 ) ) ;
#18106 = CIRCLE ( 'NONE', #15633, 44.99999999999998579 ) ;
#18107 = DIRECTION ( 'NONE',  ( 1.000000000000000000, 0.000000000000000000, 0.000000000000000000 ) ) ;
#18108 = DIRECTION ( 'NONE',  ( 0.000000000000000000, -0.9702957262759939194, -0.2419218955996776110 ) ) ;
#18109 = ADVANCED_FACE ( 'NONE', ( #16973 ), #12095, .F. ) ;
#18110 = CARTESIAN_POINT ( 'NONE',  ( 10.00000000000000888, 0.000000000000000000, 0.000000000000000000 ) ) ;
#18111 = ADVANCED_FACE ( 'NONE', ( #18848 ), #8791, .F. ) ;
#18112 = ADVANCED_FACE ( 'NONE', ( #8569 ), #20506, .F. ) ;
#18113 = CYLINDRICAL_SURFACE ( 'NONE', #4470, 88.00000000000000000 ) ;
#18114 = ORIENTED_EDGE ( 'NONE', *, *, #21246, .F. ) ;
#18115 = ADVANCED_FACE ( 'NONE', ( #19065 ), #20291, .F. ) ;
#18116 = CIRCLE ( 'NONE', #17051, 11.99999999999999822 ) ;
#18117 = ORIENTED_EDGE ( 'NONE', *, *, #17178, .F. ) ;
#18118 = ORIENTED_EDGE ( 'NONE', *, *, #17851, .T. ) ;
#18119 = AXIS2_PLACEMENT_3D ( 'NONE', #5149, #5681, #19056 ) ;
#18120 = AXIS2_PLACEMENT_3D ( 'NONE', #9681, #6834, #18654 ) ;
#18121 = ORIENTED_EDGE ( 'NONE', *, *, #13637, .F. ) ;
#18122 = ORIENTED_EDGE ( 'NONE', *, *, #4441, .T. ) ;
#18123 = ADVANCED_FACE ( 'NONE', ( #18742 ), #15625, .T. ) ;
#18124 = LINE ( 'NONE', #18239, #994 ) ;
#18125 = ORIENTED_EDGE ( 'NONE', *, *, #18958, .T. ) ;
#18126 = DIRECTION ( 'NONE',  ( 0.000000000000000000, 0.000000000000000000, 1.000000000000000000 ) ) ;
#18127 = CARTESIAN_POINT ( 'NONE',  ( 0.000000000000000000, 86.66425444033919234, 32.33793443156426406 ) ) ;
#18128 = EDGE_CURVE ( 'NONE', #14785, #3387, #14734, .T. ) ;
#18129 = CIRCLE ( 'NONE', #2598, 92.50099999999999056 ) ;
#18130 = DIRECTION ( 'NONE',  ( 1.000000000000000000, 0.000000000000000000, 0.000000000000000000 ) ) ;
#18131 = CARTESIAN_POINT ( 'NONE',  ( -7.500000000000000000, 0.000000000000000000, 3.000000000000000000 ) ) ;
#18132 = DIRECTION ( 'NONE',  ( 0.000000000000000000, 0.000000000000000000, 1.000000000000000000 ) ) ;
#18133 = EDGE_CURVE ( 'NONE', #14602, #1536, #2730, .T. ) ;
#18134 = CARTESIAN_POINT ( 'NONE',  ( 10.00000000000000000, 0.000000000000000000, 0.000000000000000000 ) ) ;
#18135 = CARTESIAN_POINT ( 'NONE',  ( 10.00000000000000000, 0.000000000000000000, 0.000000000000000000 ) ) ;
#18136 = CIRCLE ( 'NONE', #15298, 44.99999999999999289 ) ;
#18137 = ORIENTED_EDGE ( 'NONE', *, *, #9594, .T. ) ;
#18138 = PRODUCT ( 'planet connector', 'planet connector', '', ( #1791 ) ) ;
#18139 = AXIS2_PLACEMENT_3D ( 'NONE', #13086, #7902, #19940 ) ;
#18140 = FACE_OUTER_BOUND ( 'NONE', #744, .T. ) ;
#18141 = EDGE_CURVE ( 'NONE', #9877, #20418, #1332, .T. ) ;
#18142 = VERTEX_POINT ( 'NONE', #13977 ) ;
#18143 = ORIENTED_EDGE ( 'NONE', *, *, #11740, .F. ) ;
#18144 = CARTESIAN_POINT ( 'NONE',  ( 0.000000000000000000, 0.000000000000000000, 0.000000000000000000 ) ) ;
#18145 = DIRECTION ( 'NONE',  ( -1.000000000000000000, 0.000000000000000000, -0.000000000000000000 ) ) ;
#18146 = AXIS2_PLACEMENT_3D ( 'NONE', #8137, #13093, #16527 ) ;
#18147 = ORIENTED_EDGE ( 'NONE', *, *, #15231, .T. ) ;
#18148 = CARTESIAN_POINT ( 'NONE',  ( 10.00000000000000000, 87.17509410653623547, 30.93441398372612738 ) ) ;
#18149 = ORIENTED_EDGE ( 'NONE', *, *, #3159, .F. ) ;
#18150 = ORIENTED_EDGE ( 'NONE', *, *, #21847, .T. ) ;
#18151 = SHAPE_DEFINITION_REPRESENTATION ( #16559, #6003 ) ;
#18152 = AXIS2_PLACEMENT_3D ( 'NONE', #11904, #21845, #6734 ) ;
#18153 = DIRECTION ( 'NONE',  ( 1.000000000000000000, 0.000000000000000000, 0.000000000000000000 ) ) ;
#18154 = ORIENTED_EDGE ( 'NONE', *, *, #16785, .T. ) ;
#18155 = DIRECTION ( 'NONE',  ( -1.000000000000000000, 0.000000000000000000, 0.000000000000000000 ) ) ;
#18156 = ADVANCED_FACE ( 'NONE', ( #7035 ), #15195, .F. ) ;
#18157 = DIRECTION ( 'NONE',  ( 0.000000000000000000, -1.000000000000000000, 0.000000000000000000 ) ) ;
#18158 = CARTESIAN_POINT ( 'NONE',  ( 0.000000000000000000, 0.000000000000000000, 25.00000000000000000 ) ) ;
#18159 = CARTESIAN_POINT ( 'NONE',  ( -10.00000000000000000, 0.000000000000000000, 0.000000000000000000 ) ) ;
#18160 = EDGE_CURVE ( 'NONE', #15532, #18176, #8384, .T. ) ;
#18161 = CARTESIAN_POINT ( 'NONE',  ( 10.00000000000000000, -1.959304526717989381, 27.42911093658674204 ) ) ;
#18162 = EDGE_CURVE ( 'NONE', #2483, #11838, #18635, .T. ) ;
#18163 = CARTESIAN_POINT ( 'NONE',  ( 10.00000000000000000, -3.786343810537388332, -27.23708136986056161 ) ) ;
#18164 = EDGE_CURVE ( 'NONE', #13661, #8013, #19322, .T. ) ;
#18165 = DIRECTION ( 'NONE',  ( -1.000000000000000000, 0.000000000000000000, 0.000000000000000000 ) ) ;
#18166 = DIRECTION ( 'NONE',  ( -1.000000000000000000, -0.000000000000000000, 0.000000000000000000 ) ) ;
#18167 = AXIS2_PLACEMENT_3D ( 'NONE', #7295, #3639, #2420 ) ;
#18168 = AXIS2_PLACEMENT_3D ( 'NONE', #16280, #1149, #6247 ) ;
#18169 = CIRCLE ( 'NONE', #12667, 44.99999999999998579 ) ;
#18170 = VERTEX_POINT ( 'NONE', #15414 ) ;
#18171 = CIRCLE ( 'NONE', #1931, 27.49900000000000233 ) ;
#18172 = ORIENTED_EDGE ( 'NONE', *, *, #4616, .F. ) ;
#18173 = VECTOR ( 'NONE', #5631, 1000.000000000000000 ) ;
#18174 = CARTESIAN_POINT ( 'NONE',  ( -10.00000000000000000, 0.000000000000000000, 0.000000000000000000 ) ) ;
#18175 = FACE_OUTER_BOUND ( 'NONE', #6360, .T. ) ;
#18176 = VERTEX_POINT ( 'NONE', #10443 ) ;
#18177 = DIRECTION ( 'NONE',  ( 0.000000000000000000, 0.000000000000000000, 1.000000000000000000 ) ) ;
#18178 = VERTEX_POINT ( 'NONE', #17193 ) ;
#18179 =( NAMED_UNIT ( * ) SI_UNIT ( $, .STERADIAN. ) SOLID_ANGLE_UNIT ( ) );
#18180 = AXIS2_PLACEMENT_3D ( 'NONE', #6302, #980, #2633 ) ;
#18181 = VERTEX_POINT ( 'NONE', #12211 ) ;
#18182 = ORIENTED_EDGE ( 'NONE', *, *, #17821, .F. ) ;
#18183 = ORIENTED_EDGE ( 'NONE', *, *, #6640, .F. ) ;
#18184 = CARTESIAN_POINT ( 'NONE',  ( -1.399999999999999911, 0.000000000000000000, 0.000000000000000000 ) ) ;
#18185 = VERTEX_POINT ( 'NONE', #18959 ) ;
#18186 = AXIS2_PLACEMENT_3D ( 'NONE', #19294, #9333, #7801 ) ;
#18187 = CIRCLE ( 'NONE', #12520, 88.00000000000000000 ) ;
#18188 = DIRECTION ( 'NONE',  ( -1.000000000000000000, -0.000000000000000000, 0.000000000000000000 ) ) ;
#18189 = DIRECTION ( 'NONE',  ( -1.000000000000000000, 0.000000000000000000, 0.000000000000000000 ) ) ;
#18190 = CYLINDRICAL_SURFACE ( 'NONE', #2665, 6.500000000000000000 ) ;
#18191 = CARTESIAN_POINT ( 'NONE',  ( 0.000000000000000000, -24.89070495400792637, 84.40647372620493627 ) ) ;
#18192 = CIRCLE ( 'NONE', #18152, 27.49900000000000233 ) ;
#18193 = CARTESIAN_POINT ( 'NONE',  ( 10.00000000000000000, 8.925965667930086056, -92.06933331948771126 ) ) ;
#18194 = LINE ( 'NONE', #6484, #6049 ) ;
#18195 = TOROIDAL_SURFACE ( 'NONE', #9009, 5.100000000000000533, 0.09999999999999971412 ) ;
#18196 = VERTEX_POINT ( 'NONE', #19162 ) ;
#18197 = DIRECTION ( 'NONE',  ( -1.000000000000000000, 0.000000000000000000, -0.000000000000000000 ) ) ;
#18198 = CARTESIAN_POINT ( 'NONE',  ( 10.00000000000000000, 0.000000000000000000, 0.000000000000000000 ) ) ;
#18199 = AXIS2_PLACEMENT_3D ( 'NONE', #9633, #18277, #1692 ) ;
#18200 = VERTEX_POINT ( 'NONE', #5802 ) ;
#18201 = AXIS2_PLACEMENT_3D ( 'NONE', #9553, #16418, #6489 ) ;
#18202 = CIRCLE ( 'NONE', #12196, 0.02570000000000176310 ) ;
#18203 = AXIS2_PLACEMENT_3D ( 'NONE', #20598, #10219, #3482 ) ;
#18204 = CARTESIAN_POINT ( 'NONE',  ( 0.000000000000000000, 0.000000000000000000, 32.00000000000000000 ) ) ;
#18205 = ORIENTED_EDGE ( 'NONE', *, *, #18430, .F. ) ;
#18206 = CARTESIAN_POINT ( 'NONE',  ( 10.00000000000000000, 0.000000000000000000, 0.000000000000000000 ) ) ;
#18207 = CARTESIAN_POINT ( 'NONE',  ( 10.00000000000000000, -25.17124263951018293, 12.69364185792209909 ) ) ;
#18208 = ORIENTED_EDGE ( 'NONE', *, *, #7876, .F. ) ;
#18209 = CARTESIAN_POINT ( 'NONE',  ( 10.00000000000000000, -37.96946988134122591, -76.11510229470897571 ) ) ;
#18210 = ORIENTED_EDGE ( 'NONE', *, *, #13564, .F. ) ;
#18211 = ORIENTED_EDGE ( 'NONE', *, *, #1999, .F. ) ;
#18212 = DIRECTION ( 'NONE',  ( 1.000000000000000000, 0.000000000000000000, 0.000000000000000000 ) ) ;
#18213 = ORIENTED_EDGE ( 'NONE', *, *, #14563, .F. ) ;
#18214 = CARTESIAN_POINT ( 'NONE',  ( 0.000000000000000000, -9.992993448021772807, 26.36019881529882980 ) ) ;
#18215 = LINE ( 'NONE', #13013, #20988 ) ;
#18216 = CARTESIAN_POINT ( 'NONE',  ( 0.000000000000000000, 12.94633825542301153, -24.26081875733320814 ) ) ;
#18217 = ADVANCED_FACE ( 'NONE', ( #6136 ), #9421, .F. ) ;
#18218 = CIRCLE ( 'NONE', #9360, 44.99999999999999289 ) ;
#18219 = DIRECTION ( 'NONE',  ( 0.000000000000000000, 4.433182216385175439E-15, -1.000000000000000000 ) ) ;
#18220 = CIRCLE ( 'NONE', #4437, 32.00000000000000000 ) ;
#18221 = DIRECTION ( 'NONE',  ( 0.000000000000000000, 0.9702957262759971391, -0.2419218955996649545 ) ) ;
#18222 = CIRCLE ( 'NONE', #3036, 44.99999999999999289 ) ;
#18223 = AXIS2_PLACEMENT_3D ( 'NONE', #10590, #537, #21193 ) ;
#18224 = CARTESIAN_POINT ( 'NONE',  ( 0.000000000000000000, 0.000000000000000000, 0.000000000000000000 ) ) ;
#18225 = DIRECTION ( 'NONE',  ( -1.000000000000000000, 0.000000000000000000, 0.000000000000000000 ) ) ;
#18226 = EDGE_CURVE ( 'NONE', #16203, #17054, #273, .T. ) ;
#18227 = CARTESIAN_POINT ( 'NONE',  ( 0.000000000000000000, 0.000000000000000000, 0.000000000000000000 ) ) ;
#18228 = CARTESIAN_POINT ( 'NONE',  ( 10.00000000000000000, -71.72924546249915068, -45.71766382684744201 ) ) ;
#18229 = DIRECTION ( 'NONE',  ( 1.000000000000000000, -0.000000000000000000, -0.000000000000000000 ) ) ;
#18230 = DIRECTION ( 'NONE',  ( 0.000000000000000000, 0.000000000000000000, -1.000000000000000000 ) ) ;
#18231 = ORIENTED_EDGE ( 'NONE', *, *, #6222, .T. ) ;
#18232 = AXIS2_PLACEMENT_3D ( 'NONE', #10494, #660, #7409 ) ;
#18233 = ORIENTED_EDGE ( 'NONE', *, *, #6326, .F. ) ;
#18234 = CIRCLE ( 'NONE', #5894, 44.99999999999998579 ) ;
#18235 = ORIENTED_EDGE ( 'NONE', *, *, #1119, .F. ) ;
#18236 = CIRCLE ( 'NONE', #17172, 44.99999999999998579 ) ;
#18237 = ORIENTED_EDGE ( 'NONE', *, *, #18013, .F. ) ;
#18238 = ORIENTED_EDGE ( 'NONE', *, *, #2307, .F. ) ;
#18239 = CARTESIAN_POINT ( 'NONE',  ( 10.00000000000000000, -1.959304526717615902, -27.42911093658677402 ) ) ;
#18240 = VERTEX_POINT ( 'NONE', #10984 ) ;
#18241 = CARTESIAN_POINT ( 'NONE',  ( 0.000000000000000000, 23.57863763525720202, 15.45211464167672588 ) ) ;
#18242 = EDGE_CURVE ( 'NONE', #13893, #15534, #12609, .T. ) ;
#18243 = EDGE_CURVE ( 'NONE', #19663, #6192, #6285, .T. ) ;
#18244 = EDGE_CURVE ( 'NONE', #1355, #21597, #9107, .T. ) ;
#18245 = DIRECTION ( 'NONE',  ( 0.000000000000000000, 0.000000000000000000, 1.000000000000000000 ) ) ;
#18246 = AXIS2_PLACEMENT_3D ( 'NONE', #1875, #7086, #3867 ) ;
#18247 = EDGE_CURVE ( 'NONE', #9731, #6423, #4864, .T. ) ;
#18248 = DIRECTION ( 'NONE',  ( -1.000000000000000000, 0.000000000000000000, 0.000000000000000000 ) ) ;
#18249 = DIRECTION ( 'NONE',  ( 0.000000000000000000, 0.000000000000000000, 1.000000000000000000 ) ) ;
#18250 = AXIS2_PLACEMENT_3D ( 'NONE', #20206, #21749, #6418 ) ;
#18251 = SURFACE_SIDE_STYLE ('',( #13144 ) ) ;
#18252 = VECTOR ( 'NONE', #14917, 1000.000000000000000 ) ;
#18253 = CARTESIAN_POINT ( 'NONE',  ( 10.00000000000000000, 25.17124263951009411, 12.69364185792227495 ) ) ;
#18254 = FACE_OUTER_BOUND ( 'NONE', #14135, .T. ) ;
#18255 = VERTEX_POINT ( 'NONE', #4023 ) ;
#18256 = CARTESIAN_POINT ( 'NONE',  ( 0.000000000000000000, -43.18649929580143976, -73.28107340219457910 ) ) ;
#18257 = ADVANCED_FACE ( 'NONE', ( #10760 ), #4151, .T. ) ;
#18258 = VERTEX_POINT ( 'NONE', #2258 ) ;
#18259 = VERTEX_POINT ( 'NONE', #19390 ) ;
#18260 = ADVANCED_FACE ( 'NONE', ( #2369 ), #12526, .F. ) ;
#18261 = DIRECTION ( 'NONE',  ( -1.000000000000000000, 0.000000000000000000, 0.000000000000000000 ) ) ;
#18262 = VERTEX_POINT ( 'NONE', #15744 ) ;
#18263 = AXIS2_PLACEMENT_3D ( 'NONE', #12766, #20853, #844 ) ;
#18264 = DIRECTION ( 'NONE',  ( -1.000000000000000000, 0.000000000000000000, 0.000000000000000000 ) ) ;
#18265 = ORIENTED_EDGE ( 'NONE', *, *, #21120, .F. ) ;
#18266 = ORIENTED_EDGE ( 'NONE', *, *, #9993, .T. ) ;
#18267 = CONTEXT_DEPENDENT_SHAPE_REPRESENTATION ( #15469, #15505 ) ;
#18268 = DIRECTION ( 'NONE',  ( -1.000000000000000000, 0.000000000000000000, -0.000000000000000000 ) ) ;
#18269 = ORIENTED_EDGE ( 'NONE', *, *, #16020, .F. ) ;
#18270 = DIRECTION ( 'NONE',  ( -1.000000000000000000, -0.000000000000000000, 0.000000000000000000 ) ) ;
#18271 = DIRECTION ( 'NONE',  ( -1.000000000000000000, 0.000000000000000000, 0.000000000000000000 ) ) ;
#18272 = ADVANCED_FACE ( 'NONE', ( #7356 ), #14090, .T. ) ;
#18273 = CARTESIAN_POINT ( 'NONE',  ( 10.00000000000000000, 84.33453774737657227, 11.08490790852157559 ) ) ;
#18274 = DIRECTION ( 'NONE',  ( 1.000000000000000000, -0.000000000000000000, -0.000000000000000000 ) ) ;
#18275 = CARTESIAN_POINT ( 'NONE',  ( 10.00000000000000000, -43.18649929580243452, 73.28107340219401067 ) ) ;
#18276 = CARTESIAN_POINT ( 'NONE',  ( -140.0000507999999968, 6.123233995736766282E-16, 5.000000000000000000 ) ) ;
#18277 = DIRECTION ( 'NONE',  ( -1.000000000000000000, -0.000000000000000000, 0.000000000000000000 ) ) ;
#18278 = DIRECTION ( 'NONE',  ( 0.000000000000000000, 0.000000000000000000, -1.000000000000000000 ) ) ;
#18279 = CIRCLE ( 'NONE', #16131, 5.633200000000004870 ) ;
#18280 = AXIS2_PLACEMENT_3D ( 'NONE', #1832, #500, #17304 ) ;
#18281 = ORIENTED_EDGE ( 'NONE', *, *, #1784, .T. ) ;
#18282 = AXIS2_PLACEMENT_3D ( 'NONE', #19983, #2960, #9685 ) ;
#18283 = EDGE_CURVE ( 'NONE', #13819, #6262, #5554, .T. ) ;
#18284 = EDGE_CURVE ( 'NONE', #9088, #7118, #2377, .T. ) ;
#18285 = AXIS2_PLACEMENT_3D ( 'NONE', #6993, #18713, #12060 ) ;
#18286 = CARTESIAN_POINT ( 'NONE',  ( 10.00000000000000000, 52.34334029047981574, -76.26670130689429072 ) ) ;
#18287 = LINE ( 'NONE', #1380, #14815 ) ;
#18288 = ORIENTED_EDGE ( 'NONE', *, *, #12818, .T. ) ;
#18289 = EDGE_CURVE ( 'NONE', #11343, #10255, #18984, .T. ) ;
#18290 = CARTESIAN_POINT ( 'NONE',  ( 0.000000000000000000, -27.82509854686807671, -4.525913221811426190 ) ) ;
#18291 = VERTEX_POINT ( 'NONE', #5912 ) ;
#18292 = EDGE_CURVE ( 'NONE', #8785, #14440, #2582, .T. ) ;
#18293 = AXIS2_PLACEMENT_3D ( 'NONE', #11958, #15588, #8744 ) ;
#18294 = VECTOR ( 'NONE', #13399, 1000.000000000000000 ) ;
#18295 = VERTEX_POINT ( 'NONE', #16063 ) ;
#18296 = DIRECTION ( 'NONE',  ( 0.000000000000000000, 0.000000000000000000, 1.000000000000000000 ) ) ;
#18297 = VERTEX_POINT ( 'NONE', #7788 ) ;
#18298 = AXIS2_PLACEMENT_3D ( 'NONE', #3136, #11538, #6577 ) ;
#18299 = ORIENTED_EDGE ( 'NONE', *, *, #13124, .T. ) ;
#18300 = DIRECTION ( 'NONE',  ( 0.000000000000000000, 0.000000000000000000, -1.000000000000000000 ) ) ;
#18301 = DIRECTION ( 'NONE',  ( 0.000000000000000000, 0.000000000000000000, 1.000000000000000000 ) ) ;
#18302 = ORIENTED_EDGE ( 'NONE', *, *, #19058, .T. ) ;
#18303 = ADVANCED_FACE ( 'NONE', ( #929 ), #7674, .F. ) ;
#18304 = CARTESIAN_POINT ( 'NONE',  ( 10.00000000000000000, -23.57863763525709189, -15.45211464167688753 ) ) ;
#18305 = DIRECTION ( 'NONE',  ( 1.000000000000000000, 0.000000000000000000, 0.000000000000000000 ) ) ;
#18306 = DIRECTION ( 'NONE',  ( -1.000000000000000000, -0.000000000000000000, 0.000000000000000000 ) ) ;
#18307 = CARTESIAN_POINT ( 'NONE',  ( 0.000000000000000000, 0.000000000000000000, 3.000000000000000000 ) ) ;
#18308 = CARTESIAN_POINT ( 'NONE',  ( 10.00000000000000000, 87.17509410653667601, -30.93441398372498341 ) ) ;
#18309 = FACE_OUTER_BOUND ( 'NONE', #18699, .T. ) ;
#18310 = UNCERTAINTY_MEASURE_WITH_UNIT (LENGTH_MEASURE( 1.000000000000000082E-05 ), #3244, 'distance_accuracy_value', 'NONE');
#18311 = ORIENTED_EDGE ( 'NONE', *, *, #4161, .T. ) ;
#18312 = CARTESIAN_POINT ( 'NONE',  ( 0.000000000000000000, 100.0000000000000000, 0.000000000000000000 ) ) ;
#18313 = AXIS2_PLACEMENT_3D ( 'NONE', #4538, #14248, #19341 ) ;
#18314 = CARTESIAN_POINT ( 'NONE',  ( 10.00000000000000000, -12.90282758292996235, 25.06465718894773431 ) ) ;
#18315 = CIRCLE ( 'NONE', #1028, 32.00000000000000000 ) ;
#18316 = ORIENTED_EDGE ( 'NONE', *, *, #973, .T. ) ;
#18317 = CIRCLE ( 'NONE', #21126, 92.50100000000000477 ) ;
#18318 = AXIS2_PLACEMENT_3D ( 'NONE', #19363, #8094, #18041 ) ;
#18319 = AXIS2_PLACEMENT_3D ( 'NONE', #21556, #16254, #9940 ) ;
#18320 = DIRECTION ( 'NONE',  ( -1.000000000000000000, -0.000000000000000000, 0.000000000000000000 ) ) ;
#18321 = ORIENTED_EDGE ( 'NONE', *, *, #908, .T. ) ;
#18322 = FACE_OUTER_BOUND ( 'NONE', #3171, .T. ) ;
#18323 = CARTESIAN_POINT ( 'NONE',  ( -1.200000000000006617, 0.000000000000000000, 0.000000000000000000 ) ) ;
#18324 = ORIENTED_EDGE ( 'NONE', *, *, #15783, .F. ) ;
#18325 = DIRECTION ( 'NONE',  ( -0.000000000000000000, 1.000000000000000000, -0.000000000000000000 ) ) ;
#18326 = ORIENTED_EDGE ( 'NONE', *, *, #11572, .F. ) ;
#18327 = VERTEX_POINT ( 'NONE', #4355 ) ;
#18328 = CIRCLE ( 'NONE', #12965, 92.50100000000000477 ) ;
#18329 = DIRECTION ( 'NONE',  ( 1.000000000000000000, 0.000000000000000000, 0.000000000000000000 ) ) ;
#18330 = VERTEX_POINT ( 'NONE', #14520 ) ;
#18331 = CYLINDRICAL_SURFACE ( 'NONE', #13027, 88.00000000000000000 ) ;
#18332 = DIRECTION ( 'NONE',  ( -1.000000000000000000, -0.000000000000000000, -0.000000000000000000 ) ) ;
#18333 = CARTESIAN_POINT ( 'NONE',  ( 0.000000000000000000, -18.31866948046784671, 26.23788002993718393 ) ) ;
#18334 = CIRCLE ( 'NONE', #14069, 44.99999999999998579 ) ;
#18335 = DIRECTION ( 'NONE',  ( 0.000000000000000000, 0.000000000000000000, 1.000000000000000000 ) ) ;
#18336 = VECTOR ( 'NONE', #10792, 1000.000000000000000 ) ;
#18337 = CIRCLE ( 'NONE', #8087, 92.50100000000000477 ) ;
#18338 = CARTESIAN_POINT ( 'NONE',  ( 0.000000000000000000, 23.10190250628833297, 89.56973317806607326 ) ) ;
#18339 = DIRECTION ( 'NONE',  ( 0.000000000000000000, 0.000000000000000000, -1.000000000000000000 ) ) ;
#18340 = LINE ( 'NONE', #6626, #8908 ) ;
#18341 = CARTESIAN_POINT ( 'NONE',  ( 0.000000000000000000, 22.77465461094674026, 15.41136296218094159 ) ) ;
#18342 = CYLINDRICAL_SURFACE ( 'NONE', #5118, 12.00000000000000000 ) ;
#18343 = DIRECTION ( 'NONE',  ( -1.000000000000000000, -0.000000000000000000, 0.000000000000000000 ) ) ;
#18344 = ORIENTED_EDGE ( 'NONE', *, *, #13363, .T. ) ;
#18345 = CARTESIAN_POINT ( 'NONE',  ( 10.00000000000000000, 41.21966518006070146, -82.80926399530243032 ) ) ;
#18346 = EDGE_CURVE ( 'NONE', #8251, #9836, #21584, .T. ) ;
#18347 = CIRCLE ( 'NONE', #14448, 44.99999999999999289 ) ;
#18348 = VERTEX_POINT ( 'NONE', #16282 ) ;
#18349 = AXIS2_PLACEMENT_3D ( 'NONE', #292, #9110, #18961 ) ;
#18350 = AXIS2_PLACEMENT_3D ( 'NONE', #13676, #20542, #13452 ) ;
#18351 = VERTEX_POINT ( 'NONE', #19712 ) ;
#18352 = VERTEX_POINT ( 'NONE', #6461 ) ;
#18353 = PRODUCT_RELATED_PRODUCT_CATEGORY ( 'part', '', ( #11423 ) ) ;
#18354 = ORIENTED_EDGE ( 'NONE', *, *, #21225, .F. ) ;
#18355 = DIRECTION ( 'NONE',  ( 1.000000000000000000, 0.000000000000000000, 0.000000000000000000 ) ) ;
#18356 = ORIENTED_EDGE ( 'NONE', *, *, #20972, .F. ) ;
#18357 = DIRECTION ( 'NONE',  ( -1.000000000000000000, -0.000000000000000000, -0.000000000000000000 ) ) ;
#18358 = CARTESIAN_POINT ( 'NONE',  ( 0.000000000000000000, 75.27139873020885830, 53.76477968147837316 ) ) ;
#18359 = FACE_OUTER_BOUND ( 'NONE', #8574, .T. ) ;
#18360 = DIRECTION ( 'NONE',  ( 0.000000000000000000, 0.000000000000000000, 1.000000000000000000 ) ) ;
#18361 = CARTESIAN_POINT ( 'NONE',  ( -1.500000000000000000, 5.453125000000000000, 0.000000000000000000 ) ) ;
#18362 = AXIS2_PLACEMENT_3D ( 'NONE', #8215, #6694, #6578 ) ;
#18363 = AXIS2_PLACEMENT_3D ( 'NONE', #15297, #8676, #16739 ) ;
#18364 = FACE_OUTER_BOUND ( 'NONE', #5054, .T. ) ;
#18365 = DIRECTION ( 'NONE',  ( 0.000000000000000000, 0.000000000000000000, 1.000000000000000000 ) ) ;
#18366 = VERTEX_POINT ( 'NONE', #11311 ) ;
#18367 = DIRECTION ( 'NONE',  ( 1.000000000000000000, 0.000000000000000000, 0.000000000000000000 ) ) ;
#18368 = EDGE_CURVE ( 'NONE', #17019, #12527, #10141, .T. ) ;
#18369 = VERTEX_POINT ( 'NONE', #13075 ) ;
#18370 = ORIENTED_EDGE ( 'NONE', *, *, #1369, .T. ) ;
#18371 = CARTESIAN_POINT ( 'NONE',  ( 10.00000000000000000, 7.619321854369911051, -26.42235673590683476 ) ) ;
#18372 = ORIENTED_EDGE ( 'NONE', *, *, #16541, .F. ) ;
#18373 = CIRCLE ( 'NONE', #21540, 44.99999999999999289 ) ;
#18374 = CARTESIAN_POINT ( 'NONE',  ( 0.000000000000000000, -84.79630770241078608, -6.691460262316255125 ) ) ;
#18375 = ORIENTED_EDGE ( 'NONE', *, *, #7863, .F. ) ;
#18376 = ORIENTED_EDGE ( 'NONE', *, *, #15830, .T. ) ;
#18377 = ITEM_DEFINED_TRANSFORMATION ( 'NONE', 'NONE', #10279,  #15567 ) ;
#18378 = DIRECTION ( 'NONE',  ( 0.000000000000000000, -0.4067366430758069806, 0.9135454576425978690 ) ) ;
#18379 = VERTEX_POINT ( 'NONE', #9534 ) ;
#18380 = DIRECTION ( 'NONE',  ( 0.000000000000000000, 0.000000000000000000, 1.000000000000000000 ) ) ;
#18381 = LINE ( 'NONE', #9956, #1137 ) ;
#18382 = EDGE_CURVE ( 'NONE', #11418, #16010, #6252, .T. ) ;
#18383 = CARTESIAN_POINT ( 'NONE',  ( 5.000000000000000888, 18.31866948046766552, 26.23788002993730828 ) ) ;
#18384 = DIRECTION ( 'NONE',  ( 0.000000000000000000, 0.000000000000000000, 1.000000000000000000 ) ) ;
#18385 = PRESENTATION_STYLE_ASSIGNMENT (( #1574 ) ) ;
#18386 = DIRECTION ( 'NONE',  ( 1.000000000000000000, -0.000000000000000000, -0.000000000000000000 ) ) ;
#18387 = ADVANCED_FACE ( 'NONE', ( #18394 ), #9871, .F. ) ;
#18388 = DIRECTION ( 'NONE',  ( 0.000000000000000000, -0.3420201433256568890, -0.9396926207859125357 ) ) ;
#18389 = CARTESIAN_POINT ( 'NONE',  ( 5.000000000000000000, 81.34229909304724515, -33.57723005635285318 ) ) ;
#18390 = ORIENTED_EDGE ( 'NONE', *, *, #4734, .T. ) ;
#18391 = ADVANCED_FACE ( 'NONE', ( #18061 ), #17956, .F. ) ;
#18392 = ADVANCED_FACE ( 'NONE', ( #16714 ), #19928, .T. ) ;
#18393 = EDGE_CURVE ( 'NONE', #3473, #13081, #8755, .T. ) ;
#18394 = FACE_OUTER_BOUND ( 'NONE', #1023, .T. ) ;
#18395 = EDGE_CURVE ( 'NONE', #10561, #17030, #7893, .T. ) ;
#18396 = CARTESIAN_POINT ( 'NONE',  ( 0.000000000000000000, 0.000000000000000000, 0.000000000000000000 ) ) ;
#18397 = ORIENTED_EDGE ( 'NONE', *, *, #20980, .T. ) ;
#18398 = CARTESIAN_POINT ( 'NONE',  ( 10.00000000000000000, 64.95266917914399585, -59.37298010462904330 ) ) ;
#18399 = ORIENTED_EDGE ( 'NONE', *, *, #4618, .T. ) ;
#18400 = SURFACE_STYLE_FILL_AREA ( #154 ) ;
#18401 = VERTEX_POINT ( 'NONE', #12968 ) ;
#18402 = DIRECTION ( 'NONE',  ( 0.000000000000000000, 0.000000000000000000, -1.000000000000000000 ) ) ;
#18403 = VERTEX_POINT ( 'NONE', #2913 ) ;
#18404 = ORIENTED_EDGE ( 'NONE', *, *, #15542, .F. ) ;
#18405 = CARTESIAN_POINT ( 'NONE',  ( 10.00000000000000000, 3.974475837766159980, -92.41557521768187655 ) ) ;
#18406 = DIRECTION ( 'NONE',  ( -1.000000000000000000, 0.000000000000000000, 0.000000000000000000 ) ) ;
#18407 = ORIENTED_EDGE ( 'NONE', *, *, #7869, .F. ) ;
#18408 = EDGE_CURVE ( 'NONE', #1529, #19408, #10862, .T. ) ;
#18409 = DIRECTION ( 'NONE',  ( 0.000000000000000000, 0.000000000000000000, -1.000000000000000000 ) ) ;
#18410 = DIRECTION ( 'NONE',  ( 0.000000000000000000, -1.680754301168640043E-14, -1.000000000000000000 ) ) ;
#18411 = DIRECTION ( 'NONE',  ( 0.000000000000000000, 0.000000000000000000, 1.000000000000000000 ) ) ;
#18412 = EDGE_CURVE ( 'NONE', #17610, #2850, #8329, .T. ) ;
#18413 = CARTESIAN_POINT ( 'NONE',  ( 10.00000000000000000, 88.70892494636740366, 26.21376805916615282 ) ) ;
#18414 = CARTESIAN_POINT ( 'NONE',  ( 10.00000000000000000, -14.02138820414853448, -83.89630571862299746 ) ) ;
#18415 = EDGE_CURVE ( 'NONE', #16952, #4620, #11933, .T. ) ;
#18416 = DIRECTION ( 'NONE',  ( 0.000000000000000000, -1.000000000000000000, 0.000000000000000000 ) ) ;
#18417 = VERTEX_POINT ( 'NONE', #1377 ) ;
#18418 = EDGE_CURVE ( 'NONE', #4497, #13650, #10158, .T. ) ;
#18419 = FACE_OUTER_BOUND ( 'NONE', #8866, .T. ) ;
#18420 = CARTESIAN_POINT ( 'NONE',  ( -90.00000000000000000, 0.000000000000000000, -115.1000000000000227 ) ) ;
#18421 = ORIENTED_EDGE ( 'NONE', *, *, #9290, .T. ) ;
#18422 = MECHANICAL_DESIGN_GEOMETRIC_PRESENTATION_REPRESENTATION (  '', ( #20866 ), #5353 ) ;
#18423 = FACE_OUTER_BOUND ( 'NONE', #1340, .T. ) ;
#18424 = VERTEX_POINT ( 'NONE', #16393 ) ;
#18425 = EDGE_CURVE ( 'NONE', #11655, #20466, #8056, .T. ) ;
#18426 = DIRECTION ( 'NONE',  ( -1.000000000000000000, 0.000000000000000000, 0.000000000000000000 ) ) ;
#18427 = CARTESIAN_POINT ( 'NONE',  ( 10.00000000000000000, 0.000000000000000000, 0.000000000000000000 ) ) ;
#18428 = ORIENTED_EDGE ( 'NONE', *, *, #12834, .F. ) ;
#18429 = CARTESIAN_POINT ( 'NONE',  ( 5.000000000000002665, -86.54587337002867287, -15.93147207947093236 ) ) ;
#18430 = EDGE_CURVE ( 'NONE', #12429, #18327, #20153, .T. ) ;
#18431 = EDGE_LOOP ( 'NONE', ( #13207, #20233 ) ) ;
#18432 = EDGE_LOOP ( 'NONE', ( #19222, #8660, #17192, #4773 ) ) ;
#18433 = DIRECTION ( 'NONE',  ( 0.000000000000000000, -0.4067366430758069806, 0.9135454576425978690 ) ) ;
#18434 = EDGE_LOOP ( 'NONE', ( #3027, #19139, #6821, #4278 ) ) ;
#18435 = DIRECTION ( 'NONE',  ( -1.000000000000000000, 0.000000000000000000, -0.000000000000000000 ) ) ;
#18436 = CARTESIAN_POINT ( 'NONE',  ( 10.00000000000000000, 72.53479564998846740, -44.42851404693280415 ) ) ;
#18437 = DIRECTION ( 'NONE',  ( 1.000000000000000000, -0.000000000000000000, -0.000000000000000000 ) ) ;
#18438 = FACE_OUTER_BOUND ( 'NONE', #11493, .T. ) ;
#18439 = EDGE_CURVE ( 'NONE', #3876, #7736, #11213, .T. ) ;
#18440 =( LENGTH_UNIT ( ) NAMED_UNIT ( * ) SI_UNIT ( .MILLI., .METRE. ) );
#18441 = DIRECTION ( 'NONE',  ( -1.000000000000000000, -0.000000000000000000, -0.000000000000000000 ) ) ;
#18442 = CARTESIAN_POINT ( 'NONE',  ( 10.00000000000000000, 85.05652083079334602, 0.7600687895874258526 ) ) ;
#18443 = ADVANCED_FACE ( 'NONE', ( #14845 ), #14740, .F. ) ;
#18444 = CARTESIAN_POINT ( 'NONE',  ( 10.00000000000000000, -61.33825423015729683, 69.23910433415923649 ) ) ;
#18445 = CARTESIAN_POINT ( 'NONE',  ( 10.00000000000000000, -66.01871308925505843, 64.79170103522997692 ) ) ;
#18446 = CARTESIAN_POINT ( 'NONE',  ( 10.00000000000000000, 28.15804365424197186, 10.64184787299392454 ) ) ;
#18447 = ORIENTED_EDGE ( 'NONE', *, *, #17706, .F. ) ;
#18448 = DIRECTION ( 'NONE',  ( 0.000000000000000000, 1.000000000000000000, -1.224646799147353207E-16 ) ) ;
#18449 = ORIENTED_EDGE ( 'NONE', *, *, #1192, .T. ) ;
#18450 = ORIENTED_EDGE ( 'NONE', *, *, #13241, .F. ) ;
#18451 = AXIS2_PLACEMENT_3D ( 'NONE', #15814, #11276, #773 ) ;
#18452 = ORIENTED_EDGE ( 'NONE', *, *, #20181, .T. ) ;
#18453 = ORIENTED_EDGE ( 'NONE', *, *, #14613, .T. ) ;
#18454 = CARTESIAN_POINT ( 'NONE',  ( 10.00000000000000000, -84.33453774737664332, 11.08490790852103380 ) ) ;
#18455 = CIRCLE ( 'NONE', #1519, 11.99999999999999822 ) ;
#18456 = ORIENTED_EDGE ( 'NONE', *, *, #18141, .T. ) ;
#18457 = DIRECTION ( 'NONE',  ( -1.000000000000000000, 0.000000000000000000, -0.000000000000000000 ) ) ;
#18459 = ADVANCED_FACE ( 'NONE', ( #20375 ), #2131, .T. ) ;
#18458 = DIRECTION ( 'NONE',  ( 1.000000000000000000, 0.000000000000000000, 0.000000000000000000 ) ) ;
#18460 = AXIS2_PLACEMENT_3D ( 'NONE', #4628, #21095, #11354 ) ;
#18461 = DIRECTION ( 'NONE',  ( -1.000000000000000000, 0.000000000000000000, -0.000000000000000000 ) ) ;
#18462 = CARTESIAN_POINT ( 'NONE',  ( 10.00000000000000000, -12.94633825542284278, 24.26081875733330406 ) ) ;
#18463 = DIRECTION ( 'NONE',  ( -1.000000000000000000, 0.000000000000000000, 0.000000000000000000 ) ) ;
#18464 = CARTESIAN_POINT ( 'NONE',  ( 10.00000000000000000, 3.786343810537573518, 27.23708136986054029 ) ) ;
#18465 = ORIENTED_EDGE ( 'NONE', *, *, #2325, .T. ) ;
#18466 = CARTESIAN_POINT ( 'NONE',  ( 10.00000000000000000, 27.48365448817206769, 0.9185515634842894572 ) ) ;
#18467 = AXIS2_PLACEMENT_3D ( 'NONE', #10921, #5962, #7612 ) ;
#18468 = AXIS2_PLACEMENT_3D ( 'NONE', #19423, #975, #16226 ) ;
#18469 = ORIENTED_EDGE ( 'NONE', *, *, #13644, .F. ) ;
#18470 = CIRCLE ( 'NONE', #11391, 11.99999999999999645 ) ;
#18471 = ORIENTED_EDGE ( 'NONE', *, *, #9433, .F. ) ;
#18472 = DIRECTION ( 'NONE',  ( 0.000000000000000000, 0.000000000000000000, 1.000000000000000000 ) ) ;
#18473 = EDGE_LOOP ( 'NONE', ( #3614, #18046, #12376, #12478 ) ) ;
#18474 = FACE_OUTER_BOUND ( 'NONE', #1981, .T. ) ;
#18475 = ORIENTED_EDGE ( 'NONE', *, *, #14089, .F. ) ;
#18476 = VERTEX_POINT ( 'NONE', #6898 ) ;
#18477 = CARTESIAN_POINT ( 'NONE',  ( 10.00000000000000000, 45.60224695560570041, 80.47900393021744492 ) ) ;
#18478 = VECTOR ( 'NONE', #15434, 1000.000000000000000 ) ;
#18479 = EDGE_LOOP ( 'NONE', ( #5169, #19064, #1881, #13978 ) ) ;
#18480 = CARTESIAN_POINT ( 'NONE',  ( 0.000000000000000000, 81.34229909304679040, 33.57723005635394742 ) ) ;
#18481 = DIRECTION ( 'NONE',  ( 1.000000000000000000, -0.000000000000000000, -0.000000000000000000 ) ) ;
#18482 = CARTESIAN_POINT ( 'NONE',  ( 10.00000000000000000, -27.00677879428973682, -80.65868421664460186 ) ) ;
#18483 = EDGE_CURVE ( 'NONE', #6607, #10149, #6300, .T. ) ;
#18484 = DIRECTION ( 'NONE',  ( 0.000000000000000000, 0.000000000000000000, -1.000000000000000000 ) ) ;
#18485 = AXIS2_PLACEMENT_3D ( 'NONE', #16760, #8368, #5053 ) ;
#18486 = DIRECTION ( 'NONE',  ( -1.000000000000000000, 0.000000000000000000, -0.000000000000000000 ) ) ;
#18487 = DIRECTION ( 'NONE',  ( 0.000000000000000000, -0.9945218953682721796, -0.1045284632676636571 ) ) ;
#18488 = FACE_OUTER_BOUND ( 'NONE', #21819, .T. ) ;
#18489 = ORIENTED_EDGE ( 'NONE', *, *, #8576, .F. ) ;
#18490 = ADVANCED_FACE ( 'NONE', ( #8543 ), #3464, .F. ) ;
#18491 = AXIS2_PLACEMENT_3D ( 'NONE', #1064, #19507, #17863 ) ;
#18492 = DIRECTION ( 'NONE',  ( -1.000000000000000000, 0.000000000000000000, 0.000000000000000000 ) ) ;
#18493 = EDGE_CURVE ( 'NONE', #14806, #9696, #1695, .T. ) ;
#18494 = AXIS2_PLACEMENT_3D ( 'NONE', #14618, #17950, #2689 ) ;
#18495 = LINE ( 'NONE', #15272, #12337 ) ;
#18496 = ORIENTED_EDGE ( 'NONE', *, *, #3650, .T. ) ;
#18497 = DIRECTION ( 'NONE',  ( -1.000000000000000000, 0.000000000000000000, 0.000000000000000000 ) ) ;
#18498 = PRODUCT_DEFINITION_SHAPE ( 'NONE', 'NONE',  #21866 ) ;
#18499 = EDGE_LOOP ( 'NONE', ( #77, #3305, #2067, #13551 ) ) ;
#18500 = AXIS2_PLACEMENT_3D ( 'NONE', #13986, #18971, #17528 ) ;
#18501 = ORIENTED_EDGE ( 'NONE', *, *, #13784, .T. ) ;
#18502 = DIRECTION ( 'NONE',  ( 1.000000000000000000, 0.000000000000000000, 0.000000000000000000 ) ) ;
#18503 = VERTEX_POINT ( 'NONE', #18929 ) ;
#18504 = VERTEX_POINT ( 'NONE', #17049 ) ;
#18505 = PLANE ( 'NONE',  #4743 ) ;
#18506 = DIRECTION ( 'NONE',  ( 0.000000000000000000, -0.9702957262759938084, -0.2419218955996777498 ) ) ;
#18507 = ORIENTED_EDGE ( 'NONE', *, *, #10970, .T. ) ;
#18508 = CIRCLE ( 'NONE', #3672, 44.99999999999999289 ) ;
#18509 = EDGE_CURVE ( 'NONE', #6423, #12565, #21109, .T. ) ;
#18510 = LINE ( 'NONE', #15287, #4039 ) ;
#18511 = CARTESIAN_POINT ( 'NONE',  ( 10.00000000000000000, 18.31866948046803145, -26.23788002993704893 ) ) ;
#18512 = EDGE_CURVE ( 'NONE', #16592, #4702, #10410, .T. ) ;
#18513 = CARTESIAN_POINT ( 'NONE',  ( 10.00000000000000000, 0.000000000000000000, 0.000000000000000000 ) ) ;
#18514 = EDGE_CURVE ( 'NONE', #5375, #21588, #15271, .T. ) ;
#18515 = DIRECTION ( 'NONE',  ( -1.000000000000000000, -0.000000000000000000, -0.000000000000000000 ) ) ;
#18516 = CARTESIAN_POINT ( 'NONE',  ( 5.000000000000000000, 68.93609746931237225, -54.69748134696388320 ) ) ;
#18517 = LINE ( 'NONE', #8237, #4623 ) ;
#18518 = ADVANCED_FACE ( 'NONE', ( #5234 ), #5124, .T. ) ;
#18519 = ORIENTED_EDGE ( 'NONE', *, *, #18512, .T. ) ;
#18520 = AXIS2_PLACEMENT_3D ( 'NONE', #4666, #16043, #11188 ) ;
#18521 = CYLINDRICAL_SURFACE ( 'NONE', #18710, 44.99999999999999289 ) ;
#18522 = DIRECTION ( 'NONE',  ( 0.000000000000000000, 0.000000000000000000, 1.000000000000000000 ) ) ;
#18523 = EDGE_LOOP ( 'NONE', ( #7141, #11863, #12090, #18118 ) ) ;
#18524 = LINE ( 'NONE', #6392, #605 ) ;
#18525 = EDGE_CURVE ( 'NONE', #11272, #15501, #10520, .T. ) ;
#18526 = ORIENTED_EDGE ( 'NONE', *, *, #10310, .T. ) ;
#18527 = CIRCLE ( 'NONE', #14634, 32.00000000000000000 ) ;
#18528 = CIRCLE ( 'NONE', #20995, 88.00000000000000000 ) ;
#18529 = DIRECTION ( 'NONE',  ( 0.000000000000000000, 0.9510565162951521989, 0.3090169943749513926 ) ) ;
#18530 = ORIENTED_EDGE ( 'NONE', *, *, #5159, .T. ) ;
#18531 = VECTOR ( 'NONE', #14553, 1000.000000000000000 ) ;
#18532 = CARTESIAN_POINT ( 'NONE',  ( -10.00000000000000000, 0.000000000000000000, 88.00000000000000000 ) ) ;
#18533 = EDGE_CURVE ( 'NONE', #4965, #16206, #19001, .T. ) ;
#18534 = VECTOR ( 'NONE', #20387, 1000.000000000000000 ) ;
#18535 = EDGE_LOOP ( 'NONE', ( #16265, #5486, #14803, #19791 ) ) ;
#18536 = ORIENTED_EDGE ( 'NONE', *, *, #11551, .F. ) ;
#18537 = ORIENTED_EDGE ( 'NONE', *, *, #14633, .T. ) ;
#18538 = CYLINDRICAL_SURFACE ( 'NONE', #17776, 44.99999999999999289 ) ;
#18539 = VERTEX_POINT ( 'NONE', #17165 ) ;
#18540 = DIRECTION ( 'NONE',  ( 0.000000000000000000, 0.000000000000000000, 1.000000000000000000 ) ) ;
#18541 = DIRECTION ( 'NONE',  ( 0.000000000000000000, 0.000000000000000000, 1.000000000000000000 ) ) ;
#18542 = CARTESIAN_POINT ( 'NONE',  ( 5.000000000000000000, 83.48638250753266732, -27.82128566055030916 ) ) ;
#18543 = FACE_OUTER_BOUND ( 'NONE', #7741, .T. ) ;
#18544 = DIRECTION ( 'NONE',  ( -1.000000000000000000, -0.000000000000000000, 0.000000000000000000 ) ) ;
#18545 = EDGE_CURVE ( 'NONE', #14663, #17231, #14749, .T. ) ;
#18546 = VECTOR ( 'NONE', #10079, 1000.000000000000000 ) ;
#18547 = CARTESIAN_POINT ( 'NONE',  ( 5.000000000000000000, 68.93609746931163329, 54.69748134696484954 ) ) ;
#18548 = CIRCLE ( 'NONE', #9341, 11.99999999999999822 ) ;
#18549 = CARTESIAN_POINT ( 'NONE',  ( 5.000000000000000000, -52.25832601289046409, -70.80301803122840454 ) ) ;
#18550 = AXIS2_PLACEMENT_3D ( 'NONE', #11541, #2915, #11652 ) ;
#18551 = VECTOR ( 'NONE', #4373, 1000.000000000000000 ) ;
#18552 = CARTESIAN_POINT ( 'NONE',  ( 10.00000000000000000, 35.34277389771654043, -85.48288328206348297 ) ) ;
#18553 = CIRCLE ( 'NONE', #12178, 44.99999999999999289 ) ;
#18554 = FACE_OUTER_BOUND ( 'NONE', #10628, .T. ) ;
#18555 = DIRECTION ( 'NONE',  ( 1.000000000000000000, -0.000000000000000000, -0.000000000000000000 ) ) ;
#18556 = EDGE_CURVE ( 'NONE', #17402, #1592, #14033, .T. ) ;
#18557 = VERTEX_POINT ( 'NONE', #3674 ) ;
#18558 =( NAMED_UNIT ( * ) SI_UNIT ( $, .STERADIAN. ) SOLID_ANGLE_UNIT ( ) );
#18559 = EDGE_LOOP ( 'NONE', ( #16178, #18745, #2002, #8049 ) ) ;
#18560 = AXIS2_PLACEMENT_3D ( 'NONE', #21703, #16729, #5022 ) ;
#18561 = LINE ( 'NONE', #3416, #649 ) ;
#18562 = EDGE_CURVE ( 'NONE', #535, #6588, #1700, .T. ) ;
#18563 = VERTEX_POINT ( 'NONE', #18606 ) ;
#18564 = ORIENTED_EDGE ( 'NONE', *, *, #3234, .T. ) ;
#18565 = CIRCLE ( 'NONE', #10421, 44.99999999999999289 ) ;
#18566 = ADVANCED_FACE ( 'NONE', ( #11858 ), #10200, .T. ) ;
#18567 = VECTOR ( 'NONE', #3487, 1000.000000000000000 ) ;
#18568 = VECTOR ( 'NONE', #2039, 1000.000000000000000 ) ;
#18569 = ADVANCED_FACE ( 'NONE', ( #18720 ), #10300, .F. ) ;
#18570 = ORIENTED_EDGE ( 'NONE', *, *, #11328, .F. ) ;
#18571 = DIRECTION ( 'NONE',  ( 0.000000000000000000, -0.06975647374413235235, 0.9975640502598237536 ) ) ;
#18572 = EDGE_LOOP ( 'NONE', ( #17742, #7467, #19840, #14971, #9258, #7419, #16956, #16673 ) ) ;
#18573 = LINE ( 'NONE', #4751, #17027 ) ;
#18574 = DIRECTION ( 'NONE',  ( 0.000000000000000000, -8.943463253924875462E-15, -1.000000000000000000 ) ) ;
#18575 = CARTESIAN_POINT ( 'NONE',  ( -10.00000000000000000, 0.000000000000000000, 0.000000000000000000 ) ) ;
#18576 = LINE ( 'NONE', #3430, #21063 ) ;
#18577 = DIRECTION ( 'NONE',  ( 1.000000000000000000, 0.000000000000000000, 0.000000000000000000 ) ) ;
#18578 = CYLINDRICAL_SURFACE ( 'NONE', #13307, 44.99999999999999289 ) ;
#18579 = CARTESIAN_POINT ( 'NONE',  ( 10.00000000000000000, 0.000000000000000000, 0.000000000000000000 ) ) ;
#18580 = ORIENTED_EDGE ( 'NONE', *, *, #8143, .F. ) ;
#18581 = VECTOR ( 'NONE', #11528, 1000.000000000000000 ) ;
#18582 = CARTESIAN_POINT ( 'NONE',  ( 10.00000000000000000, -75.27139873020921357, 53.76477968147791131 ) ) ;
#18583 = CIRCLE ( 'NONE', #21741, 6.866799999999992465 ) ;
#18584 = ORIENTED_EDGE ( 'NONE', *, *, #14877, .T. ) ;
#18585 = ORIENTED_EDGE ( 'NONE', *, *, #19302, .F. ) ;
#18586 = DIRECTION ( 'NONE',  ( -1.000000000000000000, -0.000000000000000000, -0.000000000000000000 ) ) ;
#18587 = ORIENTED_EDGE ( 'NONE', *, *, #9895, .T. ) ;
#18588 = CARTESIAN_POINT ( 'NONE',  ( 0.000000000000000000, 0.000000000000000000, 0.000000000000000000 ) ) ;
#18589 = ORIENTED_EDGE ( 'NONE', *, *, #14796, .T. ) ;
#18590 = ORIENTED_EDGE ( 'NONE', *, *, #785, .F. ) ;
#18591 = FACE_OUTER_BOUND ( 'NONE', #16317, .T. ) ;
#18592 = VECTOR ( 'NONE', #7690, 1000.000000000000000 ) ;
#18593 = ORIENTED_EDGE ( 'NONE', *, *, #3297, .F. ) ;
#18594 = AXIS2_PLACEMENT_3D ( 'NONE', #16003, #17902, #10929 ) ;
#18595 = FACE_OUTER_BOUND ( 'NONE', #16649, .T. ) ;
#18596 = CARTESIAN_POINT ( 'NONE',  ( 10.00000000000000000, -35.34277389771592226, 85.48288328206373876 ) ) ;
#18597 = CYLINDRICAL_SURFACE ( 'NONE', #4527, 32.00000000000000000 ) ;
#18598 = LINE ( 'NONE', #20250, #7993 ) ;
#18599 = FACE_OUTER_BOUND ( 'NONE', #1658, .T. ) ;
#18600 = CYLINDRICAL_SURFACE ( 'NONE', #21690, 10.49999999999999822 ) ;
#18601 = DIRECTION ( 'NONE',  ( -1.000000000000000000, -0.000000000000000000, 0.000000000000000000 ) ) ;
#18602 = ORIENTED_EDGE ( 'NONE', *, *, #11740, .T. ) ;
#18603 = AXIS2_PLACEMENT_3D ( 'NONE', #18253, #18463, #4760 ) ;
#18604 = CIRCLE ( 'NONE', #13662, 88.00000000000000000 ) ;
#18605 = CIRCLE ( 'NONE', #1319, 88.00000000000000000 ) ;
#18606 = CARTESIAN_POINT ( 'NONE',  ( 0.000000000000000000, -78.80192417387952730, 39.16958956249271040 ) ) ;
#18607 = DIRECTION ( 'NONE',  ( 0.000000000000000000, 0.000000000000000000, 1.000000000000000000 ) ) ;
#18608 = VERTEX_POINT ( 'NONE', #13734 ) ;
#18609 = EDGE_CURVE ( 'NONE', #18016, #15910, #2344, .T. ) ;
#18610 = CYLINDRICAL_SURFACE ( 'NONE', #7250, 44.99999999999999289 ) ;
#18611 = ORIENTED_EDGE ( 'NONE', *, *, #20801, .F. ) ;
#18612 = FILL_AREA_STYLE_COLOUR ( '', #4286 ) ;
#18613 = ORIENTED_EDGE ( 'NONE', *, *, #6102, .T. ) ;
#18614 = LINE ( 'NONE', #20270, #14575 ) ;
#18615 = ORIENTED_EDGE ( 'NONE', *, *, #11895, .T. ) ;
#18616 = VERTEX_POINT ( 'NONE', #17600 ) ;
#18617 = LINE ( 'NONE', #18405, #2257 ) ;
#18618 = CARTESIAN_POINT ( 'NONE',  ( 0.000000000000000000, 0.000000000000000000, 0.000000000000000000 ) ) ;
#18619 = ADVANCED_FACE ( 'NONE', ( #12496 ), #7330, .F. ) ;
#18620 = ORIENTED_EDGE ( 'NONE', *, *, #16764, .F. ) ;
#18621 = AXIS2_PLACEMENT_3D ( 'NONE', #2524, #7729, #17350 ) ;
#18622 = DIRECTION ( 'NONE',  ( -1.000000000000000000, 0.000000000000000000, 0.000000000000000000 ) ) ;
#18623 = CARTESIAN_POINT ( 'NONE',  ( 5.000000000000000000, 67.00000000000000000, 15.00000000000000000 ) ) ;
#18624 = AXIS2_PLACEMENT_3D ( 'NONE', #17403, #3595, #15304 ) ;
#18625 = DIRECTION ( 'NONE',  ( 0.000000000000000000, -7.093091546216279124E-15, 1.000000000000000000 ) ) ;
#18626 = CARTESIAN_POINT ( 'NONE',  ( 10.00000000000000000, -27.48365448817207479, 0.9185515634840949462 ) ) ;
#18627 = VECTOR ( 'NONE', #15108, 1000.000000000000000 ) ;
#18628 = DIRECTION ( 'NONE',  ( 0.000000000000000000, 0.000000000000000000, -1.000000000000000000 ) ) ;
#18629 = CARTESIAN_POINT ( 'NONE',  ( 10.00000000000000000, 46.93287725819874368, -70.94007663282398823 ) ) ;
#18630 = CIRCLE ( 'NONE', #21438, 5.000000000000000000 ) ;
#18631 = ORIENTED_EDGE ( 'NONE', *, *, #5662, .T. ) ;
#18632 = CARTESIAN_POINT ( 'NONE',  ( 10.00000000000000000, -92.32475887865419395, -5.707354816231494432 ) ) ;
#18633 = PLANE ( 'NONE',  #10438 ) ;
#18634 = ORIENTED_EDGE ( 'NONE', *, *, #2337, .F. ) ;
#18635 = LINE ( 'NONE', #287, #21799 ) ;
#18636 = ORIENTED_EDGE ( 'NONE', *, *, #4059, .F. ) ;
#18637 = AXIS2_PLACEMENT_3D ( 'NONE', #6041, #5817, #19501 ) ;
#18638 = AXIS2_PLACEMENT_3D ( 'NONE', #21251, #6123, #2806 ) ;
#18639 = DIRECTION ( 'NONE',  ( 0.000000000000000000, 0.000000000000000000, -1.000000000000000000 ) ) ;
#18640 = ADVANCED_FACE ( 'NONE', ( #4321 ), #692, .T. ) ;
#18641 = ADVANCED_FACE ( 'NONE', ( #17701 ), #5887, .F. ) ;
#18642 = CIRCLE ( 'NONE', #20041, 27.49900000000000233 ) ;
#18643 = DIRECTION ( 'NONE',  ( 1.000000000000000000, -0.000000000000000000, -0.000000000000000000 ) ) ;
#18644 = ORIENTED_EDGE ( 'NONE', *, *, #3089, .T. ) ;
#18645 = CARTESIAN_POINT ( 'NONE',  ( 0.000000000000000000, -81.55207211302094095, 24.17537951050038814 ) ) ;
#18646 = ADVANCED_FACE ( 'NONE', ( #20902 ), #14058, .T. ) ;
#18647 = EDGE_LOOP ( 'NONE', ( #14574, #19339, #20660, #8259 ) ) ;
#18648 = ORIENTED_EDGE ( 'NONE', *, *, #8749, .T. ) ;
#18649 = VERTEX_POINT ( 'NONE', #7435 ) ;
#18650 = ORIENTED_EDGE ( 'NONE', *, *, #9866, .T. ) ;
#18651 = VECTOR ( 'NONE', #16139, 1000.000000000000000 ) ;
#18652 = DIRECTION ( 'NONE',  ( 0.000000000000000000, 0.000000000000000000, 1.000000000000000000 ) ) ;
#18653 = LINE ( 'NONE', #20310, #11090 ) ;
#18654 = DIRECTION ( 'NONE',  ( 0.000000000000000000, 0.8987940462991680368, -0.4383711467890751279 ) ) ;
#18655 = CYLINDRICAL_SURFACE ( 'NONE', #14285, 6.728125000000022560 ) ;
#18656 = DIRECTION ( 'NONE',  ( 1.000000000000000000, 0.000000000000000000, 0.000000000000000000 ) ) ;
#18657 = EDGE_CURVE ( 'NONE', #15964, #16742, #997, .T. ) ;
#18658 = AXIS2_PLACEMENT_3D ( 'NONE', #14577, #21318, #6201 ) ;
#18659 = AXIS2_PLACEMENT_3D ( 'NONE', #2292, #17549, #7279 ) ;
#18660 = DIRECTION ( 'NONE',  ( 1.000000000000000000, 0.000000000000000000, 0.000000000000000000 ) ) ;
#18661 = LINE ( 'NONE', #13230, #7504 ) ;
#18662 = CIRCLE ( 'NONE', #9112, 11.99999999999999822 ) ;
#18663 = AXIS2_PLACEMENT_3D ( 'NONE', #6545, #16473, #11614 ) ;
#18664 = ADVANCED_FACE ( 'NONE', ( #16032 ), #10955, .F. ) ;
#18665 = DIRECTION ( 'NONE',  ( -1.000000000000000000, -0.000000000000000000, -0.000000000000000000 ) ) ;
#18666 = DIRECTION ( 'NONE',  ( 1.000000000000000000, 0.000000000000000000, 0.000000000000000000 ) ) ;
#18667 = DIRECTION ( 'NONE',  ( 1.000000000000000000, 0.000000000000000000, 0.000000000000000000 ) ) ;
#18668 = ORIENTED_EDGE ( 'NONE', *, *, #13462, .F. ) ;
#18669 = EDGE_CURVE ( 'NONE', #9349, #18403, #9181, .T. ) ;
#18670 = DIRECTION ( 'NONE',  ( -1.000000000000000000, 0.000000000000000000, -0.000000000000000000 ) ) ;
#18671 = EDGE_CURVE ( 'NONE', #2869, #15286, #9097, .T. ) ;
#18672 = ORIENTED_EDGE ( 'NONE', *, *, #6950, .F. ) ;
#18673 = FACE_OUTER_BOUND ( 'NONE', #16285, .T. ) ;
#18674 = ORIENTED_EDGE ( 'NONE', *, *, #9163, .T. ) ;
#18675 = AXIS2_PLACEMENT_3D ( 'NONE', #20545, #19102, #8606 ) ;
#18676 = EDGE_CURVE ( 'NONE', #20112, #8941, #17924, .T. ) ;
#18677 = ORIENTED_EDGE ( 'NONE', *, *, #12834, .T. ) ;
#18678 = AXIS2_PLACEMENT_3D ( 'NONE', #14779, #10005, #1413 ) ;
#18679 = CIRCLE ( 'NONE', #3841, 0.02569999999999482421 ) ;
#18680 = ORIENTED_EDGE ( 'NONE', *, *, #15535, .F. ) ;
#18681 = DIRECTION ( 'NONE',  ( 1.000000000000000000, 0.000000000000000000, 0.000000000000000000 ) ) ;
#18682 = ORIENTED_EDGE ( 'NONE', *, *, #16757, .F. ) ;
#18683 = DIRECTION ( 'NONE',  ( -1.000000000000000000, 0.000000000000000000, -0.000000000000000000 ) ) ;
#18684 = FILL_AREA_STYLE ('',( #5737 ) ) ;
#18685 = EDGE_CURVE ( 'NONE', #4587, #13603, #17375, .T. ) ;
#18686 = CARTESIAN_POINT ( 'NONE',  ( 0.000000000000000000, -21.98203405400967014, 17.64965094506536403 ) ) ;
#18687 =( NAMED_UNIT ( * ) PLANE_ANGLE_UNIT ( ) SI_UNIT ( $, .RADIAN. ) );
#18688 = CARTESIAN_POINT ( 'NONE',  ( 0.000000000000000000, 0.000000000000000000, 0.000000000000000000 ) ) ;
#18689 = EDGE_CURVE ( 'NONE', #6588, #16623, #9817, .T. ) ;
#18690 = CARTESIAN_POINT ( 'NONE',  ( 10.00000000000000000, 92.32475887865426500, 5.707354816230855832 ) ) ;
#18691 = DIRECTION ( 'NONE',  ( -1.000000000000000000, -0.000000000000000000, -0.000000000000000000 ) ) ;
#18692 = CIRCLE ( 'NONE', #2106, 12.00000000000000000 ) ;
#18693 = CIRCLE ( 'NONE', #20107, 88.00000000000000000 ) ;
#18694 = AXIS2_PLACEMENT_3D ( 'NONE', #183, #6934, #13654 ) ;
#18695 = ORIENTED_EDGE ( 'NONE', *, *, #14861, .F. ) ;
#18696 = VECTOR ( 'NONE', #10675, 1000.000000000000000 ) ;
#18697 = EDGE_CURVE ( 'NONE', #20540, #6613, #21125, .T. ) ;
#18698 = DIRECTION ( 'NONE',  ( -1.000000000000000000, 0.000000000000000000, 0.000000000000000000 ) ) ;
#18699 = EDGE_LOOP ( 'NONE', ( #14681, #7340, #644, #14702 ) ) ;
#18700 = EDGE_LOOP ( 'NONE', ( #4953, #7282, #20471, #401 ) ) ;
#18701 = DIRECTION ( 'NONE',  ( -1.000000000000000000, -0.000000000000000000, 0.000000000000000000 ) ) ;
#18702 = EDGE_CURVE ( 'NONE', #6010, #15453, #7532, .T. ) ;
#18703 = ORIENTED_EDGE ( 'NONE', *, *, #21592, .F. ) ;
#18704 = DIRECTION ( 'NONE',  ( -1.000000000000000000, -0.000000000000000000, -0.000000000000000000 ) ) ;
#18705 = ORIENTED_EDGE ( 'NONE', *, *, #395, .T. ) ;
#18706 = ORIENTED_EDGE ( 'NONE', *, *, #13009, .T. ) ;
#18707 = CARTESIAN_POINT ( 'NONE',  ( 6.123233995736766282E-16, -5.000000000000000000, 3.000000000000002665 ) ) ;
#18708 = ORIENTED_EDGE ( 'NONE', *, *, #17458, .T. ) ;
#18709 = AXIS2_PLACEMENT_3D ( 'NONE', #8651, #370, #7437 ) ;
#18710 = AXIS2_PLACEMENT_3D ( 'NONE', #1828, #5035, #11992 ) ;
#18711 = FACE_OUTER_BOUND ( 'NONE', #14336, .T. ) ;
#18712 = DIRECTION ( 'NONE',  ( 1.000000000000000000, 0.000000000000000000, 0.000000000000000000 ) ) ;
#18713 = DIRECTION ( 'NONE',  ( 1.000000000000000000, 0.000000000000000000, 0.000000000000000000 ) ) ;
#18714 = CARTESIAN_POINT ( 'NONE',  ( 0.000000000000000000, -69.74988376404053270, 53.65588238863315240 ) ) ;
#18715 = DIRECTION ( 'NONE',  ( -1.000000000000000000, -0.000000000000000000, 0.000000000000000000 ) ) ;
#18716 = DIRECTION ( 'NONE',  ( 0.000000000000000000, -0.9271838545667832054, -0.3746065934159226729 ) ) ;
#18717 = CARTESIAN_POINT ( 'NONE',  ( 10.00000000000000000, -74.74361964203200159, -40.60271866773624083 ) ) ;
#18718 = ORIENTED_EDGE ( 'NONE', *, *, #21534, .F. ) ;
#18719 = ADVANCED_FACE ( 'NONE', ( #8966, #6005 ), #3999, .T. ) ;
#18720 = FACE_OUTER_BOUND ( 'NONE', #11154, .T. ) ;
#18721 = DIRECTION ( 'NONE',  ( 0.000000000000000000, 0.000000000000000000, -1.000000000000000000 ) ) ;
#18722 = ORIENTED_EDGE ( 'NONE', *, *, #1192, .F. ) ;
#18723 = CARTESIAN_POINT ( 'NONE',  ( 10.00000000000000000, -23.10190250628773967, -89.56973317806621537 ) ) ;
#18724 = ORIENTED_EDGE ( 'NONE', *, *, #17010, .T. ) ;
#18725 = EDGE_LOOP ( 'NONE', ( #10793, #15154, #20514, #7625 ) ) ;
#18726 = FACE_OUTER_BOUND ( 'NONE', #5907, .T. ) ;
#18727 = EDGE_LOOP ( 'NONE', ( #2820, #15329 ) ) ;
#18728 = EDGE_LOOP ( 'NONE', ( #19, #14720 ) ) ;
#18729 = DIRECTION ( 'NONE',  ( 1.000000000000000000, 0.000000000000000000, 0.000000000000000000 ) ) ;
#18730 = DIRECTION ( 'NONE',  ( 0.000000000000000000, -0.5299192642331944647, -0.8480480961564325071 ) ) ;
#18731 = CYLINDRICAL_SURFACE ( 'NONE', #10515, 44.99999999999998579 ) ;
#18732 = CARTESIAN_POINT ( 'NONE',  ( 0.000000000000000000, 9.366510754379232750, 25.85466064925429208 ) ) ;
#18733 = AXIS2_PLACEMENT_3D ( 'NONE', #8152, #1183, #21190 ) ;
#18734 = FACE_OUTER_BOUND ( 'NONE', #7414, .T. ) ;
#18735 = CARTESIAN_POINT ( 'NONE',  ( 0.000000000000000000, -46.93287725819829603, 70.94007663282431508 ) ) ;
#18736 = DIRECTION ( 'NONE',  ( -1.000000000000000000, -0.000000000000000000, 0.000000000000000000 ) ) ;
#18737 = VERTEX_POINT ( 'NONE', #5556 ) ;
#18738 = DIRECTION ( 'NONE',  ( 0.000000000000000000, 0.000000000000000000, 1.000000000000000000 ) ) ;
#18739 = VECTOR ( 'NONE', #14764, 1000.000000000000000 ) ;
#18740 = CARTESIAN_POINT ( 'NONE',  ( 0.000000000000000000, 74.39348546125125949, -54.97312363261338675 ) ) ;
#18741 = ORIENTED_EDGE ( 'NONE', *, *, #7436, .T. ) ;
#18742 = FACE_OUTER_BOUND ( 'NONE', #13689, .T. ) ;
#18743 = VERTEX_POINT ( 'NONE', #19461 ) ;
#18744 = CARTESIAN_POINT ( 'NONE',  ( 10.00000000000000000, -1.592605004252988898, 28.14575649959894221 ) ) ;
#18745 = ORIENTED_EDGE ( 'NONE', *, *, #20412, .T. ) ;
#18746 = ORIENTED_EDGE ( 'NONE', *, *, #254, .T. ) ;
#18747 = ORIENTED_EDGE ( 'NONE', *, *, #48, .T. ) ;
#18748 = ORIENTED_EDGE ( 'NONE', *, *, #5997, .T. ) ;
#18749 = FACE_OUTER_BOUND ( 'NONE', #10933, .T. ) ;
#18750 = ORIENTED_EDGE ( 'NONE', *, *, #562, .T. ) ;
#18751 = CARTESIAN_POINT ( 'NONE',  ( 10.00000000000000000, 0.000000000000000000, 0.000000000000000000 ) ) ;
#18752 = DIRECTION ( 'NONE',  ( 0.000000000000000000, 8.866364432770347722E-15, -1.000000000000000000 ) ) ;
#18753 = DIRECTION ( 'NONE',  ( -1.000000000000000000, 0.000000000000000000, 0.000000000000000000 ) ) ;
#18754 = CYLINDRICAL_SURFACE ( 'NONE', #13945, 44.99999999999999289 ) ;
#18755 = CARTESIAN_POINT ( 'NONE',  ( -1.129531546211690385, 0.000000000000000000, -6.887500000000022382 ) ) ;
#18756 = CARTESIAN_POINT ( 'NONE',  ( -90.00000000000000000, 0.000000000000000000, 0.000000000000000000 ) ) ;
#18757 = VECTOR ( 'NONE', #20500, 1000.000000000000227 ) ;
#18758 = EDGE_CURVE ( 'NONE', #16476, #21231, #19702, .T. ) ;
#18759 = DIRECTION ( 'NONE',  ( 0.000000000000000000, -1.000000000000000000, 0.000000000000000000 ) ) ;
#18760 = CARTESIAN_POINT ( 'NONE',  ( 0.000000000000000000, 0.000000000000000000, 0.000000000000000000 ) ) ;
#18761 = MECHANICAL_DESIGN_GEOMETRIC_PRESENTATION_REPRESENTATION (  '', ( #2519 ), #3582 ) ;
#18762 = ORIENTED_EDGE ( 'NONE', *, *, #18395, .T. ) ;
#18763 = CARTESIAN_POINT ( 'NONE',  ( 10.00000000000000000, 62.44821182181184582, -68.23969402963440700 ) ) ;
#18764 = CARTESIAN_POINT ( 'NONE',  ( -7.395799999999999486, 0.000000000000000000, 0.000000000000000000 ) ) ;
#18765 = EDGE_CURVE ( 'NONE', #17309, #16790, #6682, .T. ) ;
#18766 = CARTESIAN_POINT ( 'NONE',  ( -90.00000000000000000, 0.000000000000000000, -6.887500000000022382 ) ) ;
#18767 = EDGE_LOOP ( 'NONE', ( #8678, #9767, #7075, #15528 ) ) ;
#18768 = CARTESIAN_POINT ( 'NONE',  ( 10.00000000000000000, 0.000000000000000000, 0.000000000000000000 ) ) ;
#18769 = ORIENTED_EDGE ( 'NONE', *, *, #21649, .F. ) ;
#18770 = DIRECTION ( 'NONE',  ( -1.000000000000000000, 0.000000000000000000, -0.000000000000000000 ) ) ;
#18771 = ORIENTED_EDGE ( 'NONE', *, *, #7548, .F. ) ;
#18772 = EDGE_CURVE ( 'NONE', #2240, #15531, #15221, .T. ) ;
#18773 = VERTEX_POINT ( 'NONE', #10258 ) ;
#18774 = AXIS2_PLACEMENT_3D ( 'NONE', #15547, #8899, #3836 ) ;
#18775 = ORIENTED_EDGE ( 'NONE', *, *, #12935, .T. ) ;
#18776 = FACE_OUTER_BOUND ( 'NONE', #6293, .T. ) ;
#18777 = ORIENTED_EDGE ( 'NONE', *, *, #4464, .F. ) ;
#18778 = DIRECTION ( 'NONE',  ( 1.000000000000000000, 0.000000000000000000, 0.000000000000000000 ) ) ;
#18779 = DIRECTION ( 'NONE',  ( 1.000000000000000000, -0.000000000000000000, -0.000000000000000000 ) ) ;
#18780 = CYLINDRICAL_SURFACE ( 'NONE', #3626, 92.50100000000000477 ) ;
#18781 = EDGE_CURVE ( 'NONE', #7767, #16203, #9111, .T. ) ;
#18782 = AXIS2_PLACEMENT_3D ( 'NONE', #18025, #2872, #1216 ) ;
#18783 = CARTESIAN_POINT ( 'NONE',  ( 10.00000000000000000, 57.06999622551897033, -66.98518889142023625 ) ) ;
#18784 = ADVANCED_FACE ( 'NONE', ( #97 ), #9510, .F. ) ;
#18785 = LINE ( 'NONE', #13810, #11900 ) ;
#18786 = CYLINDRICAL_SURFACE ( 'NONE', #18167, 32.00000000000000000 ) ;
#18787 = EDGE_CURVE ( 'NONE', #13543, #13174, #16363, .T. ) ;
#18788 = LINE ( 'NONE', #20657, #11177 ) ;
#18789 = CARTESIAN_POINT ( 'NONE',  ( 10.00000000000000000, 31.15801000616942673, -79.14775961996359399 ) ) ;
#18790 = EDGE_CURVE ( 'NONE', #1972, #16720, #12936, .T. ) ;
#18791 = ORIENTED_EDGE ( 'NONE', *, *, #6465, .F. ) ;
#18792 = DIRECTION ( 'NONE',  ( 0.000000000000000000, 0.9702957262759972501, -0.2419218955996647880 ) ) ;
#18793 = ORIENTED_EDGE ( 'NONE', *, *, #41, .F. ) ;
#18794 = VERTEX_POINT ( 'NONE', #19796 ) ;
#18795 = ADVANCED_FACE ( 'NONE', ( #6849, #10148 ), #1651, .T. ) ;
#18796 = CARTESIAN_POINT ( 'NONE',  ( 10.00000000000000000, 75.27139873020885830, 53.76477968147838027 ) ) ;
#18797 = ORIENTED_EDGE ( 'NONE', *, *, #7043, .T. ) ;
#18798 = ORIENTED_EDGE ( 'NONE', *, *, #2160, .T. ) ;
#18799 = CIRCLE ( 'NONE', #17031, 44.99999999999999289 ) ;
#18800 = EDGE_CURVE ( 'NONE', #13983, #9606, #12822, .T. ) ;
#18801 = DIRECTION ( 'NONE',  ( 0.000000000000000000, 1.224646799147354933E-16, 1.000000000000000000 ) ) ;
#18802 = ORIENTED_EDGE ( 'NONE', *, *, #18949, .F. ) ;
#18803 = FACE_OUTER_BOUND ( 'NONE', #8174, .T. ) ;
#18804 = ADVANCED_FACE ( 'NONE', ( #18673 ), #4442, .F. ) ;
#18805 = AXIS2_PLACEMENT_3D ( 'NONE', #434, #7081, #340 ) ;
#18806 = CARTESIAN_POINT ( 'NONE',  ( 0.000000000000000000, 0.000000000000000000, 0.000000000000000000 ) ) ;
#18807 = CARTESIAN_POINT ( 'NONE',  ( 0.000000000000000000, -21.65267340503309512, 89.93106657554424999 ) ) ;
#18808 = CYLINDRICAL_SURFACE ( 'NONE', #15050, 45.00000000000000000 ) ;
#18809 = CYLINDRICAL_SURFACE ( 'NONE', #21659, 44.99999999999999289 ) ;
#18810 = LINE ( 'NONE', #13833, #20102 ) ;
#18811 = DIRECTION ( 'NONE',  ( -1.000000000000000000, -0.000000000000000000, -0.000000000000000000 ) ) ;
#18812 = AXIS2_PLACEMENT_3D ( 'NONE', #12041, #3637, #20654 ) ;
#18813 = CIRCLE ( 'NONE', #20914, 92.50100000000000477 ) ;
#18814 = EDGE_CURVE ( 'NONE', #12744, #5595, #17001, .T. ) ;
#18815 = ORIENTED_EDGE ( 'NONE', *, *, #5639, .T. ) ;
#18816 = CIRCLE ( 'NONE', #1524, 5.453125000000000000 ) ;
#18817 = CARTESIAN_POINT ( 'NONE',  ( 10.00000000000000000, 0.000000000000000000, 0.000000000000000000 ) ) ;
#18818 = ADVANCED_FACE ( 'NONE', ( #4553, #13573 ), #6747, .F. ) ;
#18819 = LINE ( 'NONE', #5558, #7069 ) ;
#18820 = CIRCLE ( 'NONE', #9269, 11.99999999999999822 ) ;
#18821 = VERTEX_POINT ( 'NONE', #20327 ) ;
#18822 = FACE_OUTER_BOUND ( 'NONE', #19644, .T. ) ;
#18823 = ADVANCED_FACE ( 'NONE', ( #14598 ), #13459, .F. ) ;
#18824 = ORIENTED_EDGE ( 'NONE', *, *, #1472, .F. ) ;
#18825 = ORIENTED_EDGE ( 'NONE', *, *, #6514, .F. ) ;
#18826 = AXIS2_PLACEMENT_3D ( 'NONE', #18735, #16852, #3589 ) ;
#18827 = CYLINDRICAL_SURFACE ( 'NONE', #13153, 27.49900000000000233 ) ;
#18828 = ORIENTED_EDGE ( 'NONE', *, *, #13658, .F. ) ;
#18829 = ORIENTED_EDGE ( 'NONE', *, *, #17033, .T. ) ;
#18830 = EDGE_CURVE ( 'NONE', #1433, #1041, #4897, .T. ) ;
#18831 = FACE_OUTER_BOUND ( 'NONE', #7537, .T. ) ;
#18832 = CYLINDRICAL_SURFACE ( 'NONE', #21257, 12.00000000000000000 ) ;
#18833 = AXIS2_PLACEMENT_3D ( 'NONE', #10240, #11789, #20516 ) ;
#18834 = EDGE_CURVE ( 'NONE', #18743, #9215, #17249, .T. ) ;
#18835 = CIRCLE ( 'NONE', #486, 104.9000000000000341 ) ;
#18836 = FACE_OUTER_BOUND ( 'NONE', #7899, .T. ) ;
#18837 = DIRECTION ( 'NONE',  ( -0.000000000000000000, -0.000000000000000000, -1.000000000000000000 ) ) ;
#18838 = DIRECTION ( 'NONE',  ( 1.000000000000000000, 0.000000000000000000, 0.000000000000000000 ) ) ;
#18839 = DIRECTION ( 'NONE',  ( 0.000000000000000000, -1.000000000000000000, 0.000000000000000000 ) ) ;
#18840 = DIRECTION ( 'NONE',  ( -1.000000000000000000, 0.000000000000000000, -0.000000000000000000 ) ) ;
#18841 = LINE ( 'NONE', #10321, #12748 ) ;
#18842 = AXIS2_PLACEMENT_3D ( 'NONE', #6836, #11907, #18866 ) ;
#18843 = EDGE_LOOP ( 'NONE', ( #11979, #8990, #16858, #19640 ) ) ;
#18844 = DIRECTION ( 'NONE',  ( -1.000000000000000000, 0.000000000000000000, -0.000000000000000000 ) ) ;
#18845 = CIRCLE ( 'NONE', #12131, 10.49999999999999822 ) ;
#18846 = ORIENTED_EDGE ( 'NONE', *, *, #7599, .F. ) ;
#18847 = CONICAL_SURFACE ( 'NONE', #840, 104.9000000000000341, 0.5675376247847546685 ) ;
#18848 = FACE_OUTER_BOUND ( 'NONE', #8919, .T. ) ;
#18849 = ORIENTED_EDGE ( 'NONE', *, *, #2998, .F. ) ;
#18850 = DIRECTION ( 'NONE',  ( -1.000000000000000000, 0.000000000000000000, 0.000000000000000000 ) ) ;
#18851 = CARTESIAN_POINT ( 'NONE',  ( 7.440711023145602176, 1.409568465818603827E-14, 115.1000000000000227 ) ) ;
#18852 = ORIENTED_EDGE ( 'NONE', *, *, #2313, .F. ) ;
#18853 = CARTESIAN_POINT ( 'NONE',  ( 5.000000000000000000, 81.83745710415276164, 32.35167097270178260 ) ) ;
#18854 = ORIENTED_EDGE ( 'NONE', *, *, #2464, .F. ) ;
#18855 = ORIENTED_EDGE ( 'NONE', *, *, #21273, .F. ) ;
#18856 = VERTEX_POINT ( 'NONE', #6080 ) ;
#18857 = CYLINDRICAL_SURFACE ( 'NONE', #1538, 11.99999999999999822 ) ;
#18858 = EDGE_LOOP ( 'NONE', ( #15068, #15226, #13900, #6362 ) ) ;
#18859 = APPLICATION_CONTEXT ( 'automotive_design' ) ;
#18860 = CARTESIAN_POINT ( 'NONE',  ( 10.00000000000000000, -57.47876254627184522, 62.70072803846370135 ) ) ;
#18861 = AXIS2_PLACEMENT_3D ( 'NONE', #9006, #12544, #15757 ) ;
#18862 = CARTESIAN_POINT ( 'NONE',  ( 10.00000000000000000, 52.34334029047875703, 76.26670130689501548 ) ) ;
#18863 = DIRECTION ( 'NONE',  ( 1.000000000000000000, 0.000000000000000000, 0.000000000000000000 ) ) ;
#18864 = CARTESIAN_POINT ( 'NONE',  ( 10.00000000000000000, 75.45728100697598961, 39.26051685139091063 ) ) ;
#18865 = PRODUCT ( 'stationary cover', 'stationary cover', '', ( #19366 ) ) ;
#18866 = DIRECTION ( 'NONE',  ( 0.000000000000000000, -0.7431448254773999063, 0.6691306063588519093 ) ) ;
#18867 = AXIS2_PLACEMENT_3D ( 'NONE', #15512, #10745, #17505 ) ;
#18868 = DIRECTION ( 'NONE',  ( 0.000000000000000000, 2.844946500601964266E-14, -1.000000000000000000 ) ) ;
#18869 = FACE_OUTER_BOUND ( 'NONE', #5016, .T. ) ;
#18870 = DIRECTION ( 'NONE',  ( 0.000000000000000000, -0.2079116908177468526, -0.9781476007338083534 ) ) ;
#18871 = ORIENTED_EDGE ( 'NONE', *, *, #9462, .T. ) ;
#18872 = DIRECTION ( 'NONE',  ( -1.000000000000000000, -0.000000000000000000, -0.000000000000000000 ) ) ;
#18873 = AXIS2_PLACEMENT_3D ( 'NONE', #10810, #5742, #5314 ) ;
#18874 = DIRECTION ( 'NONE',  ( 0.000000000000000000, -0.5877852522924797984, 0.8090169943749425663 ) ) ;
#18875 = CIRCLE ( 'NONE', #21686, 6.728125000000022560 ) ;
#18876 = LINE ( 'NONE', #7275, #16483 ) ;
#18877 = ORIENTED_EDGE ( 'NONE', *, *, #1373, .T. ) ;
#18878 = DIRECTION ( 'NONE',  ( 0.000000000000000000, 0.000000000000000000, -1.000000000000000000 ) ) ;
#18879 = ORIENTED_EDGE ( 'NONE', *, *, #856, .F. ) ;
#18880 = CARTESIAN_POINT ( 'NONE',  ( 10.00000000000000000, -84.12297548659729785, 12.59025161326973397 ) ) ;
#18881 = CIRCLE ( 'NONE', #21003, 9.999999999999998224 ) ;
#18882 = VERTEX_POINT ( 'NONE', #11810 ) ;
#18883 = ORIENTED_EDGE ( 'NONE', *, *, #14989, .T. ) ;
#18884 = EDGE_CURVE ( 'NONE', #21244, #11867, #18561, .T. ) ;
#18885 = ORIENTED_EDGE ( 'NONE', *, *, #6637, .T. ) ;
#18886 = LINE ( 'NONE', #3629, #20441 ) ;
#18887 = DIRECTION ( 'NONE',  ( -1.000000000000000000, -0.000000000000000000, -0.000000000000000000 ) ) ;
#18888 = CARTESIAN_POINT ( 'NONE',  ( 10.00000000000000000, -0.6021240089803571172, 31.99433460282944708 ) ) ;
#18889 = CIRCLE ( 'NONE', #14653, 104.9000000000000341 ) ;
#18890 = CARTESIAN_POINT ( 'NONE',  ( 5.000000000000002665, 73.32282170386913833, -48.65967342042704757 ) ) ;
#18891 = EDGE_CURVE ( 'NONE', #6765, #9927, #20763, .T. ) ;
#18892 = UNCERTAINTY_MEASURE_WITH_UNIT (LENGTH_MEASURE( 1.000000000000000082E-05 ), #14064, 'distance_accuracy_value', 'NONE');
#18893 = VECTOR ( 'NONE', #1572, 1000.000000000000000 ) ;
#18894 = CARTESIAN_POINT ( 'NONE',  ( 10.00000000000000000, 0.000000000000000000, 0.000000000000000000 ) ) ;
#18895 = DIRECTION ( 'NONE',  ( -1.000000000000000000, -0.000000000000000000, -0.000000000000000000 ) ) ;
#18896 = CYLINDRICAL_SURFACE ( 'NONE', #13208, 92.50100000000000477 ) ;
#18897 = AXIS2_PLACEMENT_3D ( 'NONE', #18436, #6408, #6508 ) ;
#18898 = DIRECTION ( 'NONE',  ( 0.000000000000000000, -2.929755203871941151E-14, -1.000000000000000000 ) ) ;
#18899 = CARTESIAN_POINT ( 'NONE',  ( 10.00000000000000000, 3.974475837766159980, -92.41557521768187655 ) ) ;
#18900 = ORIENTED_EDGE ( 'NONE', *, *, #9430, .T. ) ;
#18901 = DIRECTION ( 'NONE',  ( -1.000000000000000000, -0.000000000000000000, 0.000000000000000000 ) ) ;
#18902 = VECTOR ( 'NONE', #15829, 1000.000000000000000 ) ;
#18903 = ORIENTED_EDGE ( 'NONE', *, *, #9020, .F. ) ;
#18904 = AXIS2_PLACEMENT_3D ( 'NONE', #3792, #11862, #12073 ) ;
#18905 = AXIS2_PLACEMENT_3D ( 'NONE', #18513, #10103, #6380 ) ;
#18906 = VERTEX_POINT ( 'NONE', #7070 ) ;
#18907 = AXIS2_PLACEMENT_3D ( 'NONE', #4311, #21226, #17802 ) ;
#18908 = CARTESIAN_POINT ( 'NONE',  ( 10.00000000000000000, 27.26034713664097353, -7.182859710736244629 ) ) ;
#18909 = ORIENTED_EDGE ( 'NONE', *, *, #2961, .T. ) ;
#18910 = EDGE_CURVE ( 'NONE', #13052, #19662, #7389, .T. ) ;
#18911 = EDGE_CURVE ( 'NONE', #21331, #16982, #15107, .T. ) ;
#18912 = EDGE_CURVE ( 'NONE', #19254, #2288, #11945, .T. ) ;
#18913 = EDGE_LOOP ( 'NONE', ( #7571, #6966, #6290, #18182 ) ) ;
#18914 = CYLINDRICAL_SURFACE ( 'NONE', #6298, 32.00000000000000000 ) ;
#18915 = EDGE_CURVE ( 'NONE', #20854, #6613, #6316, .T. ) ;
#18916 = ORIENTED_EDGE ( 'NONE', *, *, #2761, .T. ) ;
#18917 = CARTESIAN_POINT ( 'NONE',  ( 0.000000000000000000, 0.000000000000000000, 0.000000000000000000 ) ) ;
#18918 = CARTESIAN_POINT ( 'NONE',  ( 10.00000000000000000, -46.89573839703219704, -79.73220629831536144 ) ) ;
#18919 = CARTESIAN_POINT ( 'NONE',  ( -123.5000000000000142, 1.512438796946981289E-14, 25.00000000000000000 ) ) ;
#18920 = DIRECTION ( 'NONE',  ( 1.000000000000000000, -0.000000000000000000, -0.000000000000000000 ) ) ;
#18921 = AXIS2_PLACEMENT_3D ( 'NONE', #17621, #600, #17830 ) ;
#18922 = DIRECTION ( 'NONE',  ( 0.000000000000000000, 0.000000000000000000, 1.000000000000000000 ) ) ;
#18923 = CARTESIAN_POINT ( 'NONE',  ( 10.00000000000000000, 0.000000000000000000, 0.000000000000000000 ) ) ;
#18924 = ADVANCED_FACE ( 'NONE', ( #9025 ), #5302, .F. ) ;
#18926 = AXIS2_PLACEMENT_3D ( 'NONE', #11345, #6616, #21411 ) ;
#18925 = DIRECTION ( 'NONE',  ( -1.000000000000000000, 0.000000000000000000, -0.000000000000000000 ) ) ;
#18927 = VERTEX_POINT ( 'NONE', #12129 ) ;
#18928 = EDGE_CURVE ( 'NONE', #9285, #12792, #17944, .T. ) ;
#18929 = CARTESIAN_POINT ( 'NONE',  ( 10.00000000000000000, -17.70753755129051754, 21.03896658273966480 ) ) ;
#18930 = DIRECTION ( 'NONE',  ( 1.000000000000000000, 0.000000000000000000, 0.000000000000000000 ) ) ;
#18931 = EDGE_LOOP ( 'NONE', ( #19044, #10935, #10366, #15383 ) ) ;
#18932 = AXIS2_PLACEMENT_3D ( 'NONE', #16566, #18555, #15114 ) ;
#18933 = ADVANCED_FACE ( 'NONE', ( #20639 ), #2184, .F. ) ;
#18934 = CARTESIAN_POINT ( 'NONE',  ( 10.00000000000000000, -23.57863763525731216, 15.45211464167656601 ) ) ;
#18935 = ORIENTED_EDGE ( 'NONE', *, *, #9205, .T. ) ;
#18936 = VECTOR ( 'NONE', #8750, 1000.000000000000000 ) ;
#18937 = CARTESIAN_POINT ( 'NONE',  ( -10.00000000000000000, 0.000000000000000000, 0.000000000000000000 ) ) ;
#18938 = ADVANCED_FACE ( 'NONE', ( #15332 ), #638, .F. ) ;
#18939 = ORIENTED_EDGE ( 'NONE', *, *, #13560, .F. ) ;
#18940 = ORIENTED_EDGE ( 'NONE', *, *, #20060, .T. ) ;
#18941 = DIRECTION ( 'NONE',  ( 1.000000000000000000, 0.000000000000000000, -0.000000000000000000 ) ) ;
#18942 = DIRECTION ( 'NONE',  ( 1.000000000000000000, 0.000000000000000000, 0.000000000000000000 ) ) ;
#18943 = FACE_OUTER_BOUND ( 'NONE', #7565, .T. ) ;
#18944 = DIRECTION ( 'NONE',  ( -1.000000000000000000, 0.000000000000000000, 0.000000000000000000 ) ) ;
#18945 = CARTESIAN_POINT ( 'NONE',  ( 10.00000000000000000, 3.728035544476225649, 84.97818067823770605 ) ) ;
#18946 = CARTESIAN_POINT ( 'NONE',  ( 10.00000000000000000, 8.134922360107273320, -84.67002113262471141 ) ) ;
#18947 = CARTESIAN_POINT ( 'NONE',  ( 10.00000000000000000, -0.6021240089799252404, -31.99433460282945063 ) ) ;
#18948 = CARTESIAN_POINT ( 'NONE',  ( -10.00000000000000000, 0.000000000000000000, 0.000000000000000000 ) ) ;
#18949 = EDGE_CURVE ( 'NONE', #9371, #6615, #4534, .T. ) ;
#18950 = AXIS2_PLACEMENT_3D ( 'NONE', #17591, #2451, #9174 ) ;
#18951 = AXIS2_PLACEMENT_3D ( 'NONE', #21069, #12887, #9453 ) ;
#18952 = VERTEX_POINT ( 'NONE', #14006 ) ;
#18953 = EDGE_CURVE ( 'NONE', #7736, #18563, #18991, .T. ) ;
#18954 = CIRCLE ( 'NONE', #6977, 44.99999999999999289 ) ;
#18955 = CARTESIAN_POINT ( 'NONE',  ( 10.00000000000000000, -1.592605004252595213, -28.14575649959895998 ) ) ;
#18956 = VERTEX_POINT ( 'NONE', #13799 ) ;
#18957 = EDGE_CURVE ( 'NONE', #16416, #5617, #216, .T. ) ;
#18958 = EDGE_CURVE ( 'NONE', #5049, #19254, #15449, .T. ) ;
#18959 = CARTESIAN_POINT ( 'NONE',  ( 0.000000000000000000, 39.87723064937119233, 83.46401306393586594 ) ) ;
#18960 = ORIENTED_EDGE ( 'NONE', *, *, #8812, .T. ) ;
#18961 = DIRECTION ( 'NONE',  ( 0.000000000000000000, 0.000000000000000000, 1.000000000000000000 ) ) ;
#18962 = DIRECTION ( 'NONE',  ( 1.000000000000000000, 0.000000000000000000, 0.000000000000000000 ) ) ;
#18963 = ORIENTED_EDGE ( 'NONE', *, *, #1396, .F. ) ;
#18964 =( NAMED_UNIT ( * ) PLANE_ANGLE_UNIT ( ) SI_UNIT ( $, .RADIAN. ) );
#18965 = CIRCLE ( 'NONE', #8380, 44.99999999999999289 ) ;
#18966 = ORIENTED_EDGE ( 'NONE', *, *, #16532, .T. ) ;
#18967 = ADVANCED_FACE ( 'NONE', ( #19196 ), #13686, .T. ) ;
#18968 = VERTEX_POINT ( 'NONE', #12353 ) ;
#18969 = AXIS2_PLACEMENT_3D ( 'NONE', #9781, #4826, #11778 ) ;
#18970 = ORIENTED_EDGE ( 'NONE', *, *, #3556, .T. ) ;
#18971 = DIRECTION ( 'NONE',  ( 1.000000000000000000, 0.000000000000000000, 0.000000000000000000 ) ) ;
#18972 = AXIS2_PLACEMENT_3D ( 'NONE', #7554, #19270, #5795 ) ;
#18973 = VERTEX_POINT ( 'NONE', #13894 ) ;
#18974 = DIRECTION ( 'NONE',  ( 0.000000000000000000, 0.000000000000000000, 1.000000000000000000 ) ) ;
#18975 = CARTESIAN_POINT ( 'NONE',  ( 10.00000000000000000, 0.000000000000000000, 0.000000000000000000 ) ) ;
#18976 = CARTESIAN_POINT ( 'NONE',  ( 10.00000000000000000, 0.000000000000000000, 0.000000000000000000 ) ) ;
#18977 = CYLINDRICAL_SURFACE ( 'NONE', #20259, 32.00000000000000000 ) ;
#18978 = LINE ( 'NONE', #10780, #21044 ) ;
#18979 = CARTESIAN_POINT ( 'NONE',  ( 10.00000000000000000, 64.66851233300799606, -55.25552418572899427 ) ) ;
#18980 = ORIENTED_EDGE ( 'NONE', *, *, #20997, .F. ) ;
#18981 = LINE ( 'NONE', #15765, #10573 ) ;
#18982 = AXIS2_PLACEMENT_3D ( 'NONE', #4778, #10185, #16934 ) ;
#18983 = CARTESIAN_POINT ( 'NONE',  ( 10.00000000000000000, 51.76708072107978609, -67.49339815138442589 ) ) ;
#18984 = CIRCLE ( 'NONE', #8040, 12.00000000000000000 ) ;
#18985 = VECTOR ( 'NONE', #1717, 1000.000000000000000 ) ;
#18986 = AXIS2_PLACEMENT_3D ( 'NONE', #11414, #1371, #8111 ) ;
#18987 = CARTESIAN_POINT ( 'NONE',  ( 0.000000000000000000, -28.15804365424196121, -1.358152127006266197 ) ) ;
#18988 = ORIENTED_EDGE ( 'NONE', *, *, #13338, .T. ) ;
#18989 = DIRECTION ( 'NONE',  ( 0.000000000000000000, 1.224646799147324364E-16, 1.000000000000000000 ) ) ;
#18990 = ORIENTED_EDGE ( 'NONE', *, *, #12702, .F. ) ;
#18991 = LINE ( 'NONE', #10475, #14771 ) ;
#18992 = ORIENTED_EDGE ( 'NONE', *, *, #21528, .T. ) ;
#18993 = AXIS2_PLACEMENT_3D ( 'NONE', #13493, #3454, #15369 ) ;
#18994 = ORIENTED_EDGE ( 'NONE', *, *, #21717, .F. ) ;
#18995 = ORIENTED_EDGE ( 'NONE', *, *, #14454, .T. ) ;
#18996 = DIRECTION ( 'NONE',  ( 1.000000000000000000, 0.000000000000000000, 0.000000000000000000 ) ) ;
#18997 = AXIS2_PLACEMENT_3D ( 'NONE', #21000, #2534, #6085 ) ;
#18998 = AXIS2_PLACEMENT_3D ( 'NONE', #17828, #5901, #14171 ) ;
#18999 = CARTESIAN_POINT ( 'NONE',  ( 0.000000000000000000, 57.53593069156472239, -72.42963261300903355 ) ) ;
#19000 = CARTESIAN_POINT ( 'NONE',  ( 10.00000000000000000, 37.96946988134172329, 76.11510229470873412 ) ) ;
#19001 = CIRCLE ( 'NONE', #2396, 11.99999999999999822 ) ;
#19002 = AXIS2_PLACEMENT_3D ( 'NONE', #6634, #20537, #8497 ) ;
#19003 = AXIS2_PLACEMENT_3D ( 'NONE', #4433, #10731, #2340 ) ;
#19004 = DIRECTION ( 'NONE',  ( -1.000000000000000000, 0.000000000000000000, 0.000000000000000000 ) ) ;
#19005 = DIRECTION ( 'NONE',  ( -1.000000000000000000, 0.000000000000000000, 0.000000000000000000 ) ) ;
#19006 = DIRECTION ( 'NONE',  ( 0.000000000000000000, 0.000000000000000000, 1.000000000000000000 ) ) ;
#19007 = CARTESIAN_POINT ( 'NONE',  ( 10.00000000000000000, -27.82509854686807671, -4.525913221811426190 ) ) ;
#19008 = CARTESIAN_POINT ( 'NONE',  ( 10.00000000000000000, 4.294029059350239486, -27.86182539015961979 ) ) ;
#19009 = FACE_OUTER_BOUND ( 'NONE', #12153, .T. ) ;
#19010 = EDGE_CURVE ( 'NONE', #16638, #18504, #5723, .T. ) ;
#19011 = ORIENTED_EDGE ( 'NONE', *, *, #6995, .F. ) ;
#19012 = DIRECTION ( 'NONE',  ( 0.000000000000000000, 0.000000000000000000, 1.000000000000000000 ) ) ;
#19013 = VERTEX_POINT ( 'NONE', #3851 ) ;
#19014 = AXIS2_PLACEMENT_3D ( 'NONE', #17927, #1235, #11288 ) ;
#19015 = ORIENTED_EDGE ( 'NONE', *, *, #8647, .T. ) ;
#19016 = AXIS2_PLACEMENT_3D ( 'NONE', #421, #10684, #12558 ) ;
#19017 = CIRCLE ( 'NONE', #8438, 92.50100000000000477 ) ;
#19018 = EDGE_CURVE ( 'NONE', #17245, #9780, #12447, .T. ) ;
#19019 = ORIENTED_EDGE ( 'NONE', *, *, #1699, .T. ) ;
#19020 = CARTESIAN_POINT ( 'NONE',  ( 0.000000000000000000, -25.17124263951000529, -12.69364185792245081 ) ) ;
#19021 = ORIENTED_EDGE ( 'NONE', *, *, #17335, .F. ) ;
#19022 = VERTEX_POINT ( 'NONE', #10794 ) ;
#19023 = CARTESIAN_POINT ( 'NONE',  ( 10.00000000000000000, -81.34229909304701778, 33.57723005635337898 ) ) ;
#19024 = VERTEX_POINT ( 'NONE', #17438 ) ;
#19025 = DIRECTION ( 'NONE',  ( 0.000000000000000000, 0.000000000000000000, 1.000000000000000000 ) ) ;
#19026 = CARTESIAN_POINT ( 'NONE',  ( 10.00000000000000000, 56.34908017029645322, -63.71789861856395731 ) ) ;
#19027 = AXIS2_PLACEMENT_3D ( 'NONE', #18860, #9194, #6944 ) ;
#19028 = CARTESIAN_POINT ( 'NONE',  ( -10.00000000000000000, 0.000000000000000000, 0.000000000000000000 ) ) ;
#19029 = AXIS2_PLACEMENT_3D ( 'NONE', #13326, #5044, #16427 ) ;
#19030 = CARTESIAN_POINT ( 'NONE',  ( 0.000000000000000000, 0.000000000000000000, 0.000000000000000000 ) ) ;
#19031 = CIRCLE ( 'NONE', #13031, 32.00000000000000000 ) ;
#19032 = CIRCLE ( 'NONE', #4939, 44.99999999999998579 ) ;
#19033 = DIRECTION ( 'NONE',  ( -1.000000000000000000, 0.000000000000000000, 0.000000000000000000 ) ) ;
#19034 = CARTESIAN_POINT ( 'NONE',  ( 10.00000000000000888, 0.000000000000000000, 0.000000000000000000 ) ) ;
#19035 = DIRECTION ( 'NONE',  ( 0.000000000000000000, 0.000000000000000000, 1.000000000000000000 ) ) ;
#19036 = EDGE_CURVE ( 'NONE', #4200, #21244, #19354, .T. ) ;
#19037 = EDGE_LOOP ( 'NONE', ( #7817, #13944, #11247, #9718 ) ) ;
#19038 = DIRECTION ( 'NONE',  ( 1.000000000000000000, 0.000000000000000000, 0.000000000000000000 ) ) ;
#19039 = VECTOR ( 'NONE', #11077, 1000.000000000000000 ) ;
#19040 = CARTESIAN_POINT ( 'NONE',  ( 0.000000000000000000, 74.74361964203228581, -40.60271866773572214 ) ) ;
#19041 = ORIENTED_EDGE ( 'NONE', *, *, #3844, .T. ) ;
#19042 = FACE_OUTER_BOUND ( 'NONE', #1937, .T. ) ;
#19043 = CIRCLE ( 'NONE', #16222, 44.99999999999999289 ) ;
#19044 = ORIENTED_EDGE ( 'NONE', *, *, #5829, .F. ) ;
#19045 = ADVANCED_FACE ( 'NONE', ( #747 ), #14218, .T. ) ;
#19046 = CYLINDRICAL_SURFACE ( 'NONE', #108, 45.00000000000000000 ) ;
#19047 = EDGE_LOOP ( 'NONE', ( #14909, #9951, #11204, #21700 ) ) ;
#19048 = ORIENTED_EDGE ( 'NONE', *, *, #12699, .F. ) ;
#19049 = DIRECTION ( 'NONE',  ( -1.000000000000000000, -0.000000000000000000, 0.000000000000000000 ) ) ;
#19050 = CARTESIAN_POINT ( 'NONE',  ( 0.000000000000000000, 0.000000000000000000, 100.0000000000000000 ) ) ;
#19051 = EDGE_CURVE ( 'NONE', #11509, #18379, #20964, .T. ) ;
#19052 = CARTESIAN_POINT ( 'NONE',  ( 10.00000000000000000, 28.15804365424197186, -1.358152127006073684 ) ) ;
#19053 = CARTESIAN_POINT ( 'NONE',  ( -1.129531546211723025, 0.000000000000000000, 0.000000000000000000 ) ) ;
#19054 = CARTESIAN_POINT ( 'NONE',  ( 10.00000000000000000, 75.87763420127832603, 44.57111876559751096 ) ) ;
#19055 = DIRECTION ( 'NONE',  ( 0.000000000000000000, 0.000000000000000000, 1.000000000000000000 ) ) ;
#19056 = DIRECTION ( 'NONE',  ( 0.000000000000000000, 0.000000000000000000, -1.000000000000000000 ) ) ;
#19057 = CYLINDRICAL_SURFACE ( 'NONE', #2783, 7.500000000000000000 ) ;
#19058 = EDGE_CURVE ( 'NONE', #17955, #6262, #19749, .T. ) ;
#19059 = EDGE_CURVE ( 'NONE', #9606, #14519, #18315, .T. ) ;
#19060 = EDGE_CURVE ( 'NONE', #8420, #21583, #8788, .T. ) ;
#19061 = ORIENTED_EDGE ( 'NONE', *, *, #9202, .T. ) ;
#19062 = CYLINDRICAL_SURFACE ( 'NONE', #5866, 45.00000000000000000 ) ;
#19063 = EDGE_CURVE ( 'NONE', #15534, #21383, #13372, .T. ) ;
#19064 = ORIENTED_EDGE ( 'NONE', *, *, #4313, .T. ) ;
#19065 = FACE_OUTER_BOUND ( 'NONE', #7184, .T. ) ;
#19066 = ORIENTED_EDGE ( 'NONE', *, *, #944, .T. ) ;
#19067 = DIRECTION ( 'NONE',  ( -1.000000000000000000, -0.000000000000000000, -0.000000000000000000 ) ) ;
#19068 = CARTESIAN_POINT ( 'NONE',  ( 5.000000000000000000, 36.39558101400249512, -80.12091913260344711 ) ) ;
#19069 = ORIENTED_EDGE ( 'NONE', *, *, #15795, .F. ) ;
#19070 = PRESENTATION_STYLE_ASSIGNMENT (( #2374 ) ) ;
#19071 = ADVANCED_FACE ( 'NONE', ( #9559 ), #19415, .F. ) ;
#19072 = EDGE_LOOP ( 'NONE', ( #12991, #8217, #16098, #10237 ) ) ;
#19073 = ORIENTED_EDGE ( 'NONE', *, *, #7160, .F. ) ;
#19074 = ORIENTED_EDGE ( 'NONE', *, *, #17361, .T. ) ;
#19075 = AXIS2_PLACEMENT_3D ( 'NONE', #10521, #8862, #12938 ) ;
#19076 = CARTESIAN_POINT ( 'NONE',  ( 0.000000000000000000, 0.000000000000000000, 0.000000000000000000 ) ) ;
#19077 = EDGE_LOOP ( 'NONE', ( #18855, #11365, #8693, #17884 ) ) ;
#19078 = EDGE_CURVE ( 'NONE', #1865, #13181, #4913, .T. ) ;
#19079 = CARTESIAN_POINT ( 'NONE',  ( 0.000000000000000000, -86.77540292929711541, 14.62974526292689426 ) ) ;
#19080 = CARTESIAN_POINT ( 'NONE',  ( -90.00000000000000000, 0.000000000000000000, 0.000000000000000000 ) ) ;
#19081 = FACE_OUTER_BOUND ( 'NONE', #47, .T. ) ;
#19082 = DIRECTION ( 'NONE',  ( -1.000000000000000000, -0.000000000000000000, 0.000000000000000000 ) ) ;
#19083 = EDGE_CURVE ( 'NONE', #5617, #11894, #18334, .T. ) ;
#19084 = DIRECTION ( 'NONE',  ( -1.000000000000000000, 0.000000000000000000, 0.000000000000000000 ) ) ;
#19085 = FACE_OUTER_BOUND ( 'NONE', #13429, .T. ) ;
#19086 = VERTEX_POINT ( 'NONE', #11012 ) ;
#19087 = DIRECTION ( 'NONE',  ( -1.000000000000000000, -0.000000000000000000, 0.000000000000000000 ) ) ;
#19088 = ADVANCED_FACE ( 'NONE', ( #5839 ), #9456, .F. ) ;
#19089 = CYLINDRICAL_SURFACE ( 'NONE', #3017, 44.99999999999999289 ) ;
#19090 = AXIS2_PLACEMENT_3D ( 'NONE', #564, #7307, #5648 ) ;
#19091 = CARTESIAN_POINT ( 'NONE',  ( 0.000000000000000000, 84.90234713953992696, -5.175025661882965089 ) ) ;
#19092 = ORIENTED_EDGE ( 'NONE', *, *, #2255, .T. ) ;
#19093 = LINE ( 'NONE', #2290, #14072 ) ;
#19094 = ORIENTED_EDGE ( 'NONE', *, *, #21225, .T. ) ;
#19095 = CARTESIAN_POINT ( 'NONE',  ( 5.000000000000000000, 31.88200538760793634, 2.745493118647104325 ) ) ;
#19096 = ORIENTED_EDGE ( 'NONE', *, *, #9884, .F. ) ;
#19097 = EDGE_LOOP ( 'NONE', ( #126, #18316, #16518, #391 ) ) ;
#19098 = VERTEX_POINT ( 'NONE', #2845 ) ;
#19099 = CARTESIAN_POINT ( 'NONE',  ( 10.00000000000000000, -88.70892494636720471, -26.21376805916674613 ) ) ;
#19100 = EDGE_CURVE ( 'NONE', #1080, #13824, #9834, .T. ) ;
#19101 = ORIENTED_EDGE ( 'NONE', *, *, #10704, .F. ) ;
#19102 = DIRECTION ( 'NONE',  ( -1.000000000000000000, 0.000000000000000000, 0.000000000000000000 ) ) ;
#19103 = CARTESIAN_POINT ( 'NONE',  ( 10.00000000000000000, 92.22057093985031884, 7.197311757040840696 ) ) ;
#19104 = DIRECTION ( 'NONE',  ( 1.000000000000000000, 0.000000000000000000, 0.000000000000000000 ) ) ;
#19105 = COLOUR_RGB ( '', 0.09019608, 0.27058824, 0.51372549) ;
#19106 = DIRECTION ( 'NONE',  ( 0.000000000000000000, -0.5877852522924797984, 0.8090169943749425663 ) ) ;
#19107 = ADVANCED_FACE ( 'NONE', ( #4612 ), #7813, .F. ) ;
#19108 = DIRECTION ( 'NONE',  ( -1.000000000000000000, 0.000000000000000000, 0.000000000000000000 ) ) ;
#19109 = CARTESIAN_POINT ( 'NONE',  ( 10.00000000000000000, -76.53853822673953289, -43.42639941457193231 ) ) ;
#19110 = CARTESIAN_POINT ( 'NONE',  ( 10.00000000000000000, -79.66702613806754130, -29.80527447819517661 ) ) ;
#19111 = DIRECTION ( 'NONE',  ( -1.000000000000000000, 0.000000000000000000, -0.000000000000000000 ) ) ;
#19112 = CYLINDRICAL_SURFACE ( 'NONE', #6333, 44.99999999999999289 ) ;
#19113 = ORIENTED_EDGE ( 'NONE', *, *, #13544, .T. ) ;
#19114 = CARTESIAN_POINT ( 'NONE',  ( 10.00000000000000000, 0.000000000000000000, 0.000000000000000000 ) ) ;
#19115 = EDGE_LOOP ( 'NONE', ( #6751, #7243, #12831, #18815 ) ) ;
#19116 = ORIENTED_EDGE ( 'NONE', *, *, #9566, .T. ) ;
#19117 = ORIENTED_EDGE ( 'NONE', *, *, #18408, .T. ) ;
#19118 = CARTESIAN_POINT ( 'NONE',  ( 0.000000000000000000, -27.26034713664092379, 4.817140289263571518 ) ) ;
#19119 = ORIENTED_EDGE ( 'NONE', *, *, #19332, .F. ) ;
#19120 = EDGE_LOOP ( 'NONE', ( #5107, #16685, #5189, #16108 ) ) ;
#19121 = EDGE_CURVE ( 'NONE', #6765, #14822, #3854, .T. ) ;
#19122 = CARTESIAN_POINT ( 'NONE',  ( 5.000000000000000000, 23.37352460145313771, -21.85585385440855788 ) ) ;
#19123 = ORIENTED_EDGE ( 'NONE', *, *, #6788, .F. ) ;
#19124 = CARTESIAN_POINT ( 'NONE',  ( 0.000000000000000000, 0.000000000000000000, 25.00000000000000000 ) ) ;
#19125 = DIRECTION ( 'NONE',  ( 0.000000000000000000, 0.000000000000000000, 1.000000000000000000 ) ) ;
#19126 = DIRECTION ( 'NONE',  ( 0.000000000000000000, 0.000000000000000000, 1.000000000000000000 ) ) ;
#19127 = DIRECTION ( 'NONE',  ( 0.000000000000000000, 0.000000000000000000, 1.000000000000000000 ) ) ;
#19128 = CARTESIAN_POINT ( 'NONE',  ( 10.00000000000000000, 16.79755869217770936, -90.96305306542237190 ) ) ;
#19129 = CYLINDRICAL_SURFACE ( 'NONE', #5502, 92.50100000000000477 ) ;
#19130 = CYLINDRICAL_SURFACE ( 'NONE', #16619, 2.799999999999996714 ) ;
#19131 = DIRECTION ( 'NONE',  ( -1.000000000000000000, -0.000000000000000000, -0.000000000000000000 ) ) ;
#19132 = VECTOR ( 'NONE', #7747, 1000.000000000000000 ) ;
#19133 = ORIENTED_EDGE ( 'NONE', *, *, #19359, .F. ) ;
#19134 = CARTESIAN_POINT ( 'NONE',  ( 10.00000000000000000, -75.27139873020847460, -53.76477968147890607 ) ) ;
#19135 = AXIS2_PLACEMENT_3D ( 'NONE', #11982, #15395, #6801 ) ;
#19136 = CIRCLE ( 'NONE', #18460, 44.99999999999999289 ) ;
#19137 = CARTESIAN_POINT ( 'NONE',  ( -10.00000000000000000, 0.000000000000000000, 0.000000000000000000 ) ) ;
#19138 = CARTESIAN_POINT ( 'NONE',  ( 2.000000000000000000, 67.00000000000000000, 15.00000000000000000 ) ) ;
#19139 = ORIENTED_EDGE ( 'NONE', *, *, #14017, .T. ) ;
#19140 = DIRECTION ( 'NONE',  ( -1.000000000000000000, -0.000000000000000000, 0.000000000000000000 ) ) ;
#19141 = ORIENTED_EDGE ( 'NONE', *, *, #12863, .F. ) ;
#19142 = CARTESIAN_POINT ( 'NONE',  ( 5.000000000000002665, -87.96697768756403946, 2.410567674970269358 ) ) ;
#19143 = AXIS2_PLACEMENT_3D ( 'NONE', #20340, #16678, #5201 ) ;
#19144 = VERTEX_POINT ( 'NONE', #12891 ) ;
#19145 = EDGE_CURVE ( 'NONE', #11314, #8172, #16903, .T. ) ;
#19146 = EDGE_LOOP ( 'NONE', ( #12444, #10210, #18695, #14545 ) ) ;
#19147 = DIRECTION ( 'NONE',  ( 1.000000000000000000, -0.000000000000000000, -0.000000000000000000 ) ) ;
#19148 = CIRCLE ( 'NONE', #16687, 44.99999999999999289 ) ;
#19149 = VECTOR ( 'NONE', #1986, 1000.000000000000000 ) ;
#19150 = DIRECTION ( 'NONE',  ( 0.000000000000000000, 0.000000000000000000, 1.000000000000000000 ) ) ;
#19151 = CARTESIAN_POINT ( 'NONE',  ( 10.00000000000000000, 67.05625154133539922, -63.71729851637743280 ) ) ;
#19152 = DIRECTION ( 'NONE',  ( 0.000000000000000000, -0.8660254037844432595, 0.4999999999999919509 ) ) ;
#19153 = DIRECTION ( 'NONE',  ( 0.000000000000000000, 0.9271838545667884235, -0.3746065934159096278 ) ) ;
#19154 = EDGE_CURVE ( 'NONE', #10029, #11398, #13015, .T. ) ;
#19155 = AXIS2_PLACEMENT_3D ( 'NONE', #3683, #19255, #9087 ) ;
#19156 = LINE ( 'NONE', #12407, #4006 ) ;
#19157 = CARTESIAN_POINT ( 'NONE',  ( 10.00000000000000000, -27.07404830566974141, 4.815694066514342175 ) ) ;
#19158 = ORIENTED_EDGE ( 'NONE', *, *, #9960, .F. ) ;
#19159 = CARTESIAN_POINT ( 'NONE',  ( 5.000000000000002665, 79.38136668499790005, -37.98155635597233726 ) ) ;
#19160 = ADVANCED_FACE ( 'NONE', ( #18089 ), #16202, .T. ) ;
#19161 = VERTEX_POINT ( 'NONE', #14333 ) ;
#19162 = CARTESIAN_POINT ( 'NONE',  ( 0.000000000000000000, 33.95793648385814123, 86.04239391578002483 ) ) ;
#19163 = ORIENTED_EDGE ( 'NONE', *, *, #4655, .F. ) ;
#19164 = CIRCLE ( 'NONE', #2568, 92.50100000000000477 ) ;
#19165 = DIRECTION ( 'NONE',  ( 0.000000000000000000, 0.000000000000000000, 1.000000000000000000 ) ) ;
#19166 = DIRECTION ( 'NONE',  ( 0.000000000000000000, 0.000000000000000000, 1.000000000000000000 ) ) ;
#19167 = ORIENTED_EDGE ( 'NONE', *, *, #12715, .T. ) ;
#19168 = CIRCLE ( 'NONE', #1195, 88.00000000000000000 ) ;
#19169 = CIRCLE ( 'NONE', #20595, 6.728125000000022560 ) ;
#19170 = ORIENTED_EDGE ( 'NONE', *, *, #5400, .T. ) ;
#19171 = ORIENTED_EDGE ( 'NONE', *, *, #21484, .F. ) ;
#19172 = EDGE_CURVE ( 'NONE', #4094, #19024, #330, .T. ) ;
#19173 = ORIENTED_EDGE ( 'NONE', *, *, #145, .F. ) ;
#19174 = ADVANCED_FACE ( 'NONE', ( #15092 ), #13106, .T. ) ;
#19175 = DIRECTION ( 'NONE',  ( 0.000000000000000000, 0.9945218953682729568, 0.1045284632676569958 ) ) ;
#19176 = CARTESIAN_POINT ( 'NONE',  ( 10.00000000000000000, -86.66425444033897918, -32.33793443156484670 ) ) ;
#19177 = EDGE_LOOP ( 'NONE', ( #2120, #5814, #21496, #21586 ) ) ;
#19178 = ADVANCED_FACE ( 'NONE', ( #11682 ), #8474, .F. ) ;
#19179 = VECTOR ( 'NONE', #19406, 1000.000000000000000 ) ;
#19180 = CARTESIAN_POINT ( 'NONE',  ( 10.00000000000000000, -60.65279801375385915, 63.75921967137595914 ) ) ;
#19181 = CARTESIAN_POINT ( 'NONE',  ( 10.00000000000000000, 0.000000000000000000, 0.000000000000000000 ) ) ;
#19182 = CARTESIAN_POINT ( 'NONE',  ( 10.00000000000000000, 0.000000000000000000, 0.000000000000000000 ) ) ;
#19183 = CARTESIAN_POINT ( 'NONE',  ( 10.00000000000000000, -2.481790431838652111, -92.46770094066596357 ) ) ;
#19184 = CARTESIAN_POINT ( 'NONE',  ( 0.000000000000000000, -21.31452625070983231, 82.34610137166113475 ) ) ;
#19185 = VECTOR ( 'NONE', #18386, 1000.000000000000000 ) ;
#19186 = ORIENTED_EDGE ( 'NONE', *, *, #12168, .F. ) ;
#19187 = DIRECTION ( 'NONE',  ( 0.000000000000000000, 0.9271838545667858700, 0.3746065934159160116 ) ) ;
#19188 = EDGE_CURVE ( 'NONE', #10476, #5352, #7379, .T. ) ;
#19189 = CARTESIAN_POINT ( 'NONE',  ( 0.000000000000000000, 79.66702613806774025, -29.80527447819464371 ) ) ;
#19190 = ADVANCED_FACE ( 'NONE', ( #1731 ), #6723, .T. ) ;
#19191 = CARTESIAN_POINT ( 'NONE',  ( 0.000000000000000000, -2.481790431839888011, 92.46770094066590673 ) ) ;
#19192 = ORIENTED_EDGE ( 'NONE', *, *, #19442, .F. ) ;
#19193 = AXIS2_PLACEMENT_3D ( 'NONE', #5680, #12629, #8981 ) ;
#19194 = DIRECTION ( 'NONE',  ( -1.000000000000000000, -0.000000000000000000, -0.000000000000000000 ) ) ;
#19195 = ORIENTED_EDGE ( 'NONE', *, *, #16380, .F. ) ;
#19196 = FACE_OUTER_BOUND ( 'NONE', #5323, .T. ) ;
#19197 = ORIENTED_EDGE ( 'NONE', *, *, #1661, .T. ) ;
#19198 = AXIS2_PLACEMENT_3D ( 'NONE', #4264, #9331, #946 ) ;
#19199 = ORIENTED_EDGE ( 'NONE', *, *, #12557, .F. ) ;
#19200 = EDGE_LOOP ( 'NONE', ( #10966, #17006, #20560, #11519 ) ) ;
#19201 = DIRECTION ( 'NONE',  ( 1.000000000000000000, 0.000000000000000000, 0.000000000000000000 ) ) ;
#19202 = VECTOR ( 'NONE', #14611, 1000.000000000000000 ) ;
#19203 = ORIENTED_EDGE ( 'NONE', *, *, #15699, .F. ) ;
#19204 = DIRECTION ( 'NONE',  ( -1.000000000000000000, 0.000000000000000000, 0.000000000000000000 ) ) ;
#19205 = EDGE_CURVE ( 'NONE', #12050, #8996, #15841, .T. ) ;
#19206 = CARTESIAN_POINT ( 'NONE',  ( 1.500000000000001332, 6.678152076600409922E-16, -5.453125000000000000 ) ) ;
#19207 = DIRECTION ( 'NONE',  ( -1.000000000000000000, -0.000000000000000000, -0.000000000000000000 ) ) ;
#19208 = CARTESIAN_POINT ( 'NONE',  ( 0.000000000000000000, -26.27606311335944511, -10.21217444509438188 ) ) ;
#19209 = CIRCLE ( 'NONE', #11099, 88.00000000000000000 ) ;
#19210 = CARTESIAN_POINT ( 'NONE',  ( -140.0000507999999968, 4.000000000000000000, 1.000000000000000000 ) ) ;
#19211 = CARTESIAN_POINT ( 'NONE',  ( 0.000000000000000000, 83.89484365856945658, -26.56417150042864961 ) ) ;
#19212 = AXIS2_PLACEMENT_3D ( 'NONE', #4306, #21002, #12483 ) ;
#19213 = CARTESIAN_POINT ( 'NONE',  ( -7.600000000000002309, 0.000000000000000000, 0.000000000000000000 ) ) ;
#19214 = DIRECTION ( 'NONE',  ( 0.000000000000000000, 1.000000000000000000, -1.224646799147353207E-16 ) ) ;
#19215 = CYLINDRICAL_SURFACE ( 'NONE', #1384, 6.728125000000022560 ) ;
#19216 = EDGE_CURVE ( 'NONE', #6772, #3550, #2799, .T. ) ;
#19217 = VECTOR ( 'NONE', #12624, 1000.000000000000000 ) ;
#19218 = EDGE_LOOP ( 'NONE', ( #16586, #14393, #20879, #11901 ) ) ;
#19219 = EDGE_CURVE ( 'NONE', #20854, #15579, #17959, .T. ) ;
#19220 = VECTOR ( 'NONE', #3632, 1000.000000000000000 ) ;
#19221 = CARTESIAN_POINT ( 'NONE',  ( -10.00000000000000000, 0.000000000000000000, 0.000000000000000000 ) ) ;
#19222 = ORIENTED_EDGE ( 'NONE', *, *, #21727, .F. ) ;
#19223 = ORIENTED_EDGE ( 'NONE', *, *, #17759, .F. ) ;
#19224 = ADVANCED_FACE ( 'NONE', ( #20185 ), #6497, .F. ) ;
#19225 = EDGE_CURVE ( 'NONE', #8085, #11265, #2429, .T. ) ;
#19226 = ORIENTED_EDGE ( 'NONE', *, *, #10037, .F. ) ;
#19227 = AXIS2_PLACEMENT_3D ( 'NONE', #16330, #12786, #5856 ) ;
#19228 = EDGE_LOOP ( 'NONE', ( #7929, #12314, #10126, #18988 ) ) ;
#19229 = ORIENTED_EDGE ( 'NONE', *, *, #21090, .F. ) ;
#19230 = CIRCLE ( 'NONE', #8997, 12.00000000000000000 ) ;
#19231 = VERTEX_POINT ( 'NONE', #2945 ) ;
#19232 = AXIS2_PLACEMENT_3D ( 'NONE', #8105, #19808, #9407 ) ;
#19233 = CYLINDRICAL_SURFACE ( 'NONE', #7698, 92.50100000000000477 ) ;
#19234 = ORIENTED_EDGE ( 'NONE', *, *, #21635, .T. ) ;
#19235 = CARTESIAN_POINT ( 'NONE',  ( 10.00000000000000000, 0.000000000000000000, 0.000000000000000000 ) ) ;
#19236 = CIRCLE ( 'NONE', #4062, 115.1000000000000227 ) ;
#19237 = DIRECTION ( 'NONE',  ( 0.000000000000000000, 0.6427876096865403621, -0.7660444431189772363 ) ) ;
#19238 = CARTESIAN_POINT ( 'NONE',  ( 10.00000000000000000, 46.93287725819779155, 70.94007663282461351 ) ) ;
#19239 = DIRECTION ( 'NONE',  ( -1.000000000000000000, -0.000000000000000000, -0.000000000000000000 ) ) ;
#19240 = LINE ( 'NONE', #5880, #12583 ) ;
#19241 = CARTESIAN_POINT ( 'NONE',  ( 0.000000000000000000, 0.000000000000000000, 3.000000000000000000 ) ) ;
#19242 = DIRECTION ( 'NONE',  ( 1.000000000000000000, 0.000000000000000000, 0.000000000000000000 ) ) ;
#19243 = DIRECTION ( 'NONE',  ( 0.000000000000000000, 1.603655480014115143E-14, -1.000000000000000000 ) ) ;
#19244 = VECTOR ( 'NONE', #14542, 1000.000000000000000 ) ;
#19245 = EDGE_LOOP ( 'NONE', ( #2846, #21669, #10524, #16078 ) ) ;
#19246 = AXIS2_PLACEMENT_3D ( 'NONE', #3898, #5453, #8970 ) ;
#19247 = CIRCLE ( 'NONE', #15343, 44.99999999999999289 ) ;
#19248 = CARTESIAN_POINT ( 'NONE',  ( -6.500000000000014211, 60.00000000000001421, 0.000000000000000000 ) ) ;
#19249 = AXIS2_PLACEMENT_3D ( 'NONE', #887, #19450, #17798 ) ;
#19250 = CARTESIAN_POINT ( 'NONE',  ( 10.00000000000000000, 0.000000000000000000, 0.000000000000000000 ) ) ;
#19251 = DIRECTION ( 'NONE',  ( 0.000000000000000000, 0.000000000000000000, 1.000000000000000000 ) ) ;
#19252 = ORIENTED_EDGE ( 'NONE', *, *, #6863, .T. ) ;
#19253 = DIRECTION ( 'NONE',  ( -1.000000000000000000, 0.000000000000000000, -0.000000000000000000 ) ) ;
#19254 = VERTEX_POINT ( 'NONE', #15199 ) ;
#19255 = DIRECTION ( 'NONE',  ( 1.000000000000000000, 0.000000000000000000, 0.000000000000000000 ) ) ;
#19256 = ORIENTED_EDGE ( 'NONE', *, *, #8776, .T. ) ;
#19257 = VECTOR ( 'NONE', #16856, 1000.000000000000000 ) ;
#19258 = ORIENTED_EDGE ( 'NONE', *, *, #13068, .F. ) ;
#19259 = DIRECTION ( 'NONE',  ( 0.000000000000000000, 0.000000000000000000, -1.000000000000000000 ) ) ;
#19260 = VECTOR ( 'NONE', #607, 1000.000000000000000 ) ;
#19261 = CIRCLE ( 'NONE', #13247, 45.00000000000000000 ) ;
#19262 = CARTESIAN_POINT ( 'NONE',  ( -10.00000000000000000, 0.000000000000000000, 0.000000000000000000 ) ) ;
#19263 = CIRCLE ( 'NONE', #563, 11.99999999999999645 ) ;
#19264 = CARTESIAN_POINT ( 'NONE',  ( 0.000000000000000000, 86.66425444033963288, -32.33793443156311298 ) ) ;
#19265 = CARTESIAN_POINT ( 'NONE',  ( 5.000000000000000000, -41.89587599971600440, 77.38692120905457728 ) ) ;
#19266 = LINE ( 'NONE', #6124, #12534 ) ;
#19267 = CYLINDRICAL_SURFACE ( 'NONE', #14978, 45.00000000000000000 ) ;
#19268 = DIRECTION ( 'NONE',  ( 0.000000000000000000, 0.000000000000000000, -1.000000000000000000 ) ) ;
#19269 = CARTESIAN_POINT ( 'NONE',  ( 0.000000000000000000, -6.063030049134865429, -31.42037024962131397 ) ) ;
#19270 = DIRECTION ( 'NONE',  ( -1.000000000000000000, -0.000000000000000000, 0.000000000000000000 ) ) ;
#19271 = ORIENTED_EDGE ( 'NONE', *, *, #4247, .T. ) ;
#19272 = LINE ( 'NONE', #10436, #11144 ) ;
#19273 = EDGE_CURVE ( 'NONE', #10208, #1972, #10191, .T. ) ;
#19274 = ORIENTED_EDGE ( 'NONE', *, *, #14760, .F. ) ;
#19275 = AXIS2_PLACEMENT_3D ( 'NONE', #20230, #116, #14922 ) ;
#19276 = CIRCLE ( 'NONE', #7624, 0.2042000000000016025 ) ;
#19277 = CARTESIAN_POINT ( 'NONE',  ( 0.000000000000000000, 0.000000000000000000, -3.000000000000000000 ) ) ;
#19278 = VERTEX_POINT ( 'NONE', #11781 ) ;
#19279 = CARTESIAN_POINT ( 'NONE',  ( -140.0000507999999968, 0.000000000000000000, 0.000000000000000000 ) ) ;
#19280 = CARTESIAN_POINT ( 'NONE',  ( 1.199999999999992628, 8.434754829127421589E-16, 6.887500000000022382 ) ) ;
#19281 = VERTEX_POINT ( 'NONE', #11570 ) ;
#19282 = EDGE_CURVE ( 'NONE', #1766, #155, #14984, .T. ) ;
#19283 =( NAMED_UNIT ( * ) SI_UNIT ( $, .STERADIAN. ) SOLID_ANGLE_UNIT ( ) );
#19284 = ORIENTED_EDGE ( 'NONE', *, *, #5385, .F. ) ;
#19285 = ORIENTED_EDGE ( 'NONE', *, *, #12658, .F. ) ;
#19286 = ORIENTED_EDGE ( 'NONE', *, *, #5833, .T. ) ;
#19287 = DIRECTION ( 'NONE',  ( 1.000000000000000000, 0.000000000000000000, 0.000000000000000000 ) ) ;
#19288 = CARTESIAN_POINT ( 'NONE',  ( 5.000000000000000000, 87.96697768756401103, 2.410567674970879981 ) ) ;
#19289 = EDGE_LOOP ( 'NONE', ( #7764, #13461, #8471, #55 ) ) ;
#19290 = AXIS2_PLACEMENT_3D ( 'NONE', #3368, #21503, #15185 ) ;
#19291 = CARTESIAN_POINT ( 'NONE',  ( 5.000000000000000000, 64.95266917914399585, -59.37298010462904330 ) ) ;
#19292 = DIRECTION ( 'NONE',  ( -1.000000000000000000, 0.000000000000000000, 0.000000000000000000 ) ) ;
#19293 = AXIS2_PLACEMENT_3D ( 'NONE', #13348, #8387, #21638 ) ;
#19294 = CARTESIAN_POINT ( 'NONE',  ( -1.114300000000000290, 8.409404640385035208E-16, 6.866799999999992465 ) ) ;
#19295 = CARTESIAN_POINT ( 'NONE',  ( 0.000000000000000000, 0.000000000000000000, 0.000000000000000000 ) ) ;
#19296 = CIRCLE ( 'NONE', #1307, 92.50100000000000477 ) ;
#19297 = CARTESIAN_POINT ( 'NONE',  ( 10.00000000000000000, 0.000000000000000000, 0.000000000000000000 ) ) ;
#19298 = ORIENTED_EDGE ( 'NONE', *, *, #2736, .T. ) ;
#19299 = DIRECTION ( 'NONE',  ( -1.000000000000000000, -0.000000000000000000, -0.000000000000000000 ) ) ;
#19300 = DIRECTION ( 'NONE',  ( 1.000000000000000000, 0.000000000000000000, 0.000000000000000000 ) ) ;
#19301 = ADVANCED_FACE ( 'NONE', ( #16865 ), #13546, .F. ) ;
#19302 = EDGE_CURVE ( 'NONE', #8524, #20998, #6330, .T. ) ;
#19303 = DIRECTION ( 'NONE',  ( -1.000000000000000000, 0.000000000000000000, 0.000000000000000000 ) ) ;
#19304 = ORIENTED_EDGE ( 'NONE', *, *, #21132, .T. ) ;
#19305 = DIRECTION ( 'NONE',  ( 0.000000000000000000, -0.9510565162951565288, 0.3090169943749382919 ) ) ;
#19306 = ORIENTED_EDGE ( 'NONE', *, *, #12692, .T. ) ;
#19307 = DIRECTION ( 'NONE',  ( 0.000000000000000000, 0.000000000000000000, -1.000000000000000000 ) ) ;
#19308 = CIRCLE ( 'NONE', #5908, 88.00000000000000000 ) ;
#19309 = ORIENTED_EDGE ( 'NONE', *, *, #14471, .T. ) ;
#19310 = VERTEX_POINT ( 'NONE', #16749 ) ;
#19311 = EDGE_LOOP ( 'NONE', ( #13773, #7386, #12561, #14632 ) ) ;
#19312 = CARTESIAN_POINT ( 'NONE',  ( 10.00000000000000000, 0.000000000000000000, 0.000000000000000000 ) ) ;
#19313 = VERTEX_POINT ( 'NONE', #8150 ) ;
#19314 = EDGE_CURVE ( 'NONE', #14440, #17955, #14432, .T. ) ;
#19315 = CARTESIAN_POINT ( 'NONE',  ( 5.000000000000000888, 31.75612719289746266, -3.943144139962234451 ) ) ;
#19316 = CARTESIAN_POINT ( 'NONE',  ( 10.00000000000000000, 0.000000000000000000, 0.000000000000000000 ) ) ;
#19317 = FACE_OUTER_BOUND ( 'NONE', #830, .T. ) ;
#19318 = CARTESIAN_POINT ( 'NONE',  ( 10.00000000000000000, 87.96697768756401103, 2.410567674970879981 ) ) ;
#19319 = EDGE_CURVE ( 'NONE', #9608, #16623, #14790, .T. ) ;
#19320 = AXIS2_PLACEMENT_3D ( 'NONE', #4367, #21270, #7797 ) ;
#19321 = CARTESIAN_POINT ( 'NONE',  ( 10.00000000000000000, -57.53593069156421791, 72.42963261300944566 ) ) ;
#19322 = CIRCLE ( 'NONE', #15787, 45.00000000000000000 ) ;
#19323 = DIRECTION ( 'NONE',  ( 0.000000000000000000, 0.000000000000000000, 1.000000000000000000 ) ) ;
#19324 = DIRECTION ( 'NONE',  ( 0.000000000000000000, 0.000000000000000000, 1.000000000000000000 ) ) ;
#19325 = AXIS2_PLACEMENT_3D ( 'NONE', #19383, #11086, #4246 ) ;
#19326 = CARTESIAN_POINT ( 'NONE',  ( 1.114299999999999846, 0.000000000000000000, 0.000000000000000000 ) ) ;
#19327 = CARTESIAN_POINT ( 'NONE',  ( 10.00000000000000000, -83.48638250753248258, 27.82128566055087049 ) ) ;
#19328 = ADVANCED_FACE ( 'NONE', ( #3598 ), #2058, .F. ) ;
#19329 = ADVANCED_FACE ( 'NONE', ( #185 ), #15417, .F. ) ;
#19330 = LINE ( 'NONE', #5861, #5525 ) ;
#19331 = VERTEX_POINT ( 'NONE', #13655 ) ;
#19332 = EDGE_CURVE ( 'NONE', #16339, #20116, #8573, .T. ) ;
#19333 = ORIENTED_EDGE ( 'NONE', *, *, #4056, .T. ) ;
#19334 = ORIENTED_EDGE ( 'NONE', *, *, #7854, .T. ) ;
#19335 = VECTOR ( 'NONE', #2494, 1000.000000000000000 ) ;
#19336 = VERTEX_POINT ( 'NONE', #20725 ) ;
#19337 = AXIS2_PLACEMENT_3D ( 'NONE', #5008, #1471, #20044 ) ;
#19338 = AXIS2_PLACEMENT_3D ( 'NONE', #20578, #15598, #12066 ) ;
#19339 = ORIENTED_EDGE ( 'NONE', *, *, #18912, .F. ) ;
#19340 = EDGE_CURVE ( 'NONE', #17373, #11314, #17082, .T. ) ;
#19341 = DIRECTION ( 'NONE',  ( 0.000000000000000000, 0.000000000000000000, 1.000000000000000000 ) ) ;
#19342 = ORIENTED_EDGE ( 'NONE', *, *, #15358, .F. ) ;
#19343 = EDGE_CURVE ( 'NONE', #13007, #3216, #8448, .T. ) ;
#19344 = CYLINDRICAL_SURFACE ( 'NONE', #13262, 92.50100000000000477 ) ;
#19345 = CARTESIAN_POINT ( 'NONE',  ( 10.00000000000000000, 83.35585896458643163, -16.94078559807864792 ) ) ;
#19346 = CARTESIAN_POINT ( 'NONE',  ( 10.00000000000000000, 84.12297548659721258, -12.59025161327029529 ) ) ;
#19347 = CARTESIAN_POINT ( 'NONE',  ( 0.000000000000000000, 0.000000000000000000, 0.000000000000000000 ) ) ;
#19348 = DIRECTION ( 'NONE',  ( -1.000000000000000000, 0.000000000000000000, -0.000000000000000000 ) ) ;
#19349 = ADVANCED_FACE ( 'NONE', ( #20409 ), #7249, .F. ) ;
#19350 = FACE_OUTER_BOUND ( 'NONE', #3199, .T. ) ;
#19351 = LINE ( 'NONE', #14376, #4832 ) ;
#19352 = DIRECTION ( 'NONE',  ( -0.000000000000000000, -0.000000000000000000, -1.000000000000000000 ) ) ;
#19353 = CIRCLE ( 'NONE', #10173, 1.100000000000003642 ) ;
#19354 = CIRCLE ( 'NONE', #312, 92.50100000000000477 ) ;
#19355 = CIRCLE ( 'NONE', #3476, 44.99999999999998579 ) ;
#19356 = ORIENTED_EDGE ( 'NONE', *, *, #2255, .F. ) ;
#19357 = CIRCLE ( 'NONE', #5978, 45.00000000000000711 ) ;
#19358 = DIRECTION ( 'NONE',  ( 1.000000000000000000, 0.000000000000000000, 0.000000000000000000 ) ) ;
#19359 = EDGE_CURVE ( 'NONE', #18649, #4329, #20509, .T. ) ;
#19360 = DIRECTION ( 'NONE',  ( 1.000000000000000000, 0.000000000000000000, 0.000000000000000000 ) ) ;
#19361 = DIRECTION ( 'NONE',  ( 0.000000000000000000, 0.9271838545667884235, -0.3746065934159096278 ) ) ;
#19362 = ORIENTED_EDGE ( 'NONE', *, *, #2208, .T. ) ;
#19363 = CARTESIAN_POINT ( 'NONE',  ( 0.000000000000000000, -28.15804365424197897, 1.358152127005888055 ) ) ;
#19364 = EDGE_LOOP ( 'NONE', ( #21485, #15584 ) ) ;
#19365 = EDGE_LOOP ( 'NONE', ( #11332, #13552, #4098, #21110 ) ) ;
#19366 = PRODUCT_CONTEXT ( 'NONE', #12070, 'mechanical' ) ;
#19367 = AXIS2_PLACEMENT_3D ( 'NONE', #14014, #20336, #539 ) ;
#19368 = DIRECTION ( 'NONE',  ( -1.000000000000000000, 0.000000000000000000, 0.000000000000000000 ) ) ;
#19369 = VERTEX_POINT ( 'NONE', #18851 ) ;
#19370 = AXIS2_PLACEMENT_3D ( 'NONE', #7710, #2618, #1074 ) ;
#19371 = VERTEX_POINT ( 'NONE', #5482 ) ;
#19372 = CARTESIAN_POINT ( 'NONE',  ( 0.000000000000000000, 19.85071254963803611, -20.01672328094512565 ) ) ;
#19373 = AXIS2_PLACEMENT_3D ( 'NONE', #17434, #14331, #19305 ) ;
#19374 = VECTOR ( 'NONE', #3189, 1000.000000000000000 ) ;
#19375 = CARTESIAN_POINT ( 'NONE',  ( 10.00000000000000000, -61.71252885873428085, 58.53847642588571887 ) ) ;
#19376 = CARTESIAN_POINT ( 'NONE',  ( 10.00000000000000000, -0.6609040254605957898, -87.99751818016876825 ) ) ;
#19377 = CYLINDRICAL_SURFACE ( 'NONE', #10155, 120.0000000000000000 ) ;
#19378 = DIRECTION ( 'NONE',  ( -1.000000000000000000, 0.000000000000000000, -0.000000000000000000 ) ) ;
#19379 = DIRECTION ( 'NONE',  ( 0.000000000000000000, 0.06975647374412555224, -0.9975640502598241977 ) ) ;
#19380 = ADVANCED_FACE ( 'NONE', ( #612 ), #8687, .F. ) ;
#19381 = CYLINDRICAL_SURFACE ( 'NONE', #10015, 7.500000000000000000 ) ;
#19382 = LINE ( 'NONE', #9413, #16419 ) ;
#19383 = CARTESIAN_POINT ( 'NONE',  ( 1.139999999999995239, 0.000000000000000000, 0.000000000000000000 ) ) ;
#19384 = ORIENTED_EDGE ( 'NONE', *, *, #14082, .F. ) ;
#19385 = DIRECTION ( 'NONE',  ( -1.000000000000000000, 0.000000000000000000, -0.000000000000000000 ) ) ;
#19386 = AXIS2_PLACEMENT_3D ( 'NONE', #2700, #2486, #10764 ) ;
#19387 = ORIENTED_EDGE ( 'NONE', *, *, #3673, .F. ) ;
#19388 = CIRCLE ( 'NONE', #348, 44.99999999999998579 ) ;
#19389 = VECTOR ( 'NONE', #13346, 1000.000000000000000 ) ;
#19390 = CARTESIAN_POINT ( 'NONE',  ( -7.500000000000000000, 0.000000000000000000, 0.000000000000000000 ) ) ;
#19391 = EDGE_LOOP ( 'NONE', ( #17257, #19119, #14818, #13606 ) ) ;
#19392 = DIRECTION ( 'NONE',  ( 0.000000000000000000, 0.000000000000000000, -1.000000000000000000 ) ) ;
#19393 = CARTESIAN_POINT ( 'NONE',  ( 0.000000000000000000, -23.62010150527279961, 84.77081340225898032 ) ) ;
#19394 = ORIENTED_EDGE ( 'NONE', *, *, #7196, .T. ) ;
#19395 = ORIENTED_EDGE ( 'NONE', *, *, #581, .F. ) ;
#19396 = EDGE_LOOP ( 'NONE', ( #19199, #6150, #20328, #2113 ) ) ;
#19397 = ORIENTED_EDGE ( 'NONE', *, *, #1230, .T. ) ;
#19398 = LINE ( 'NONE', #12426, #8943 ) ;
#19399 = DIRECTION ( 'NONE',  ( 0.000000000000000000, 0.000000000000000000, 1.000000000000000000 ) ) ;
#19400 = VERTEX_POINT ( 'NONE', #16977 ) ;
#19401 = CARTESIAN_POINT ( 'NONE',  ( 5.000000000000002665, 86.77540292929722909, -14.62974526292624944 ) ) ;
#19402 = CARTESIAN_POINT ( 'NONE',  ( 10.00000000000000000, -9.646732466565913100, 84.51112348751846071 ) ) ;
#19403 = CARTESIAN_POINT ( 'NONE',  ( 10.00000000000000000, 0.000000000000000000, 0.000000000000000000 ) ) ;
#19404 = CIRCLE ( 'NONE', #15521, 44.99999999999999289 ) ;
#19405 = AXIS2_PLACEMENT_3D ( 'NONE', #16303, #1172, #13097 ) ;
#19406 = DIRECTION ( 'NONE',  ( -1.000000000000000000, 0.000000000000000000, 0.000000000000000000 ) ) ;
#19407 = CARTESIAN_POINT ( 'NONE',  ( 0.000000000000000000, 52.96496548042942010, -66.55750800669305534 ) ) ;
#19408 = VERTEX_POINT ( 'NONE', #5271 ) ;
#19409 = CARTESIAN_POINT ( 'NONE',  ( 10.00000000000000000, 30.24235385705252099, -10.45944707835077381 ) ) ;
#19410 = CARTESIAN_POINT ( 'NONE',  ( 10.00000000000000000, -91.49386717542212466, -13.61276130277086693 ) ) ;
#19411 = CARTESIAN_POINT ( 'NONE',  ( 10.00000000000000000, 0.000000000000000000, 0.000000000000000000 ) ) ;
#19412 = VERTEX_POINT ( 'NONE', #7134 ) ;
#19413 = CARTESIAN_POINT ( 'NONE',  ( 7.395799999999999486, 0.000000000000000000, 0.000000000000000000 ) ) ;
#19414 = ORIENTED_EDGE ( 'NONE', *, *, #17543, .T. ) ;
#19415 = CYLINDRICAL_SURFACE ( 'NONE', #9128, 92.50100000000000477 ) ;
#19416 = VERTEX_POINT ( 'NONE', #8995 ) ;
#19417 = ORIENTED_EDGE ( 'NONE', *, *, #18346, .F. ) ;
#19418 = VERTEX_POINT ( 'NONE', #7038 ) ;
#19419 = PLANE ( 'NONE',  #10046 ) ;
#19420 = ORIENTED_EDGE ( 'NONE', *, *, #14846, .F. ) ;
#19421 = CARTESIAN_POINT ( 'NONE',  ( 10.00000000000000000, -82.02147376274642454, -42.76579056660944644 ) ) ;
#19422 = DIRECTION ( 'NONE',  ( -1.000000000000000000, 0.000000000000000000, -0.000000000000000000 ) ) ;
#19423 = CARTESIAN_POINT ( 'NONE',  ( 0.000000000000000000, 36.60317927562682883, -76.78148674856727496 ) ) ;
#19424 = EDGE_CURVE ( 'NONE', #9177, #535, #15857, .T. ) ;
#19425 = DIRECTION ( 'NONE',  ( 1.000000000000000000, 0.000000000000000000, 0.000000000000000000 ) ) ;
#19426 = LINE ( 'NONE', #21602, #819 ) ;
#19427 = LINE ( 'NONE', #4290, #3772 ) ;
#19428 = CARTESIAN_POINT ( 'NONE',  ( 0.000000000000000000, 0.000000000000000000, 0.000000000000000000 ) ) ;
#19429 = CIRCLE ( 'NONE', #6396, 12.00000000000000178 ) ;
#19430 = ADVANCED_FACE ( 'NONE', ( #1835 ), #10447, .T. ) ;
#19431 = CARTESIAN_POINT ( 'NONE',  ( 10.00000000000000000, 15.25521607131206459, 23.70650506194175478 ) ) ;
#19432 = CARTESIAN_POINT ( 'NONE',  ( 10.00000000000000000, -61.33825423015638734, -69.23910433416007493 ) ) ;
#19433 = DIRECTION ( 'NONE',  ( 0.000000000000000000, 0.000000000000000000, 1.000000000000000000 ) ) ;
#19434 = EDGE_CURVE ( 'NONE', #10449, #20563, #2447, .T. ) ;
#19435 = ORIENTED_EDGE ( 'NONE', *, *, #20681, .F. ) ;
#19436 = ORIENTED_EDGE ( 'NONE', *, *, #11228, .T. ) ;
#19437 = VERTEX_POINT ( 'NONE', #12324 ) ;
#19438 = ORIENTED_EDGE ( 'NONE', *, *, #13563, .F. ) ;
#19439 =( GEOMETRIC_REPRESENTATION_CONTEXT ( 3 ) GLOBAL_UNCERTAINTY_ASSIGNED_CONTEXT ( ( #9893 ) ) GLOBAL_UNIT_ASSIGNED_CONTEXT ( ( #8797, #5807, #6144 ) ) REPRESENTATION_CONTEXT ( 'NONE', 'WORKASPACE' ) );
#19440 = ORIENTED_EDGE ( 'NONE', *, *, #12813, .F. ) ;
#19441 = DIRECTION ( 'NONE',  ( -1.000000000000000000, 0.000000000000000000, -0.000000000000000000 ) ) ;
#19442 = EDGE_CURVE ( 'NONE', #1794, #5152, #17308, .T. ) ;
#19443 = ORIENTED_EDGE ( 'NONE', *, *, #11741, .F. ) ;
#19444 = FACE_OUTER_BOUND ( 'NONE', #13155, .T. ) ;
#19445 = EDGE_CURVE ( 'NONE', #21566, #589, #18693, .T. ) ;
#19446 = ADVANCED_FACE ( 'NONE', ( #15748 ), #14093, .T. ) ;
#19447 = FACE_OUTER_BOUND ( 'NONE', #8915, .T. ) ;
#19448 = LINE ( 'NONE', #4426, #19132 ) ;
#19449 = ADVANCED_FACE ( 'NONE', ( #9536 ), #11097, .T. ) ;
#19450 = DIRECTION ( 'NONE',  ( -1.000000000000000000, 0.000000000000000000, 0.000000000000000000 ) ) ;
#19451 = CARTESIAN_POINT ( 'NONE',  ( 10.00000000000000000, 56.35896156215049047, -73.34918167666251065 ) ) ;
#19452 = CARTESIAN_POINT ( 'NONE',  ( 10.00000000000000000, -3.786343810537759147, 27.23708136986050832 ) ) ;
#19453 = DIRECTION ( 'NONE',  ( 1.000000000000000000, 0.000000000000000000, 0.000000000000000000 ) ) ;
#19454 = CARTESIAN_POINT ( 'NONE',  ( 10.00000000000000000, 0.000000000000000000, 0.000000000000000000 ) ) ;
#19455 = CARTESIAN_POINT ( 'NONE',  ( 10.00000000000000000, 0.000000000000000000, 0.000000000000000000 ) ) ;
#19456 = VECTOR ( 'NONE', #13758, 1000.000000000000000 ) ;
#19457 = ORIENTED_EDGE ( 'NONE', *, *, #7824, .F. ) ;
#19458 = CARTESIAN_POINT ( 'NONE',  ( 10.00000000000000000, 12.46320060045762013, -29.47318494484016327 ) ) ;
#19459 = EDGE_CURVE ( 'NONE', #2267, #17431, #347, .T. ) ;
#19460 = ORIENTED_EDGE ( 'NONE', *, *, #15492, .T. ) ;
#19461 = CARTESIAN_POINT ( 'NONE',  ( 0.000000000000000000, -24.73395913766455578, -12.01774797440602427 ) ) ;
#19462 = ADVANCED_FACE ( 'NONE', ( #5805 ), #16067, .F. ) ;
#19463 = CARTESIAN_POINT ( 'NONE',  ( -5.000000000000000000, 8.660254037844385522, 15.00000000000000000 ) ) ;
#19464 = ORIENTED_EDGE ( 'NONE', *, *, #12443, .F. ) ;
#19465 = CARTESIAN_POINT ( 'NONE',  ( 0.000000000000000000, 0.000000000000000000, 0.000000000000000000 ) ) ;
#19466 = VERTEX_POINT ( 'NONE', #19393 ) ;
#19467 = ORIENTED_EDGE ( 'NONE', *, *, #9462, .F. ) ;
#19468 = CARTESIAN_POINT ( 'NONE',  ( 0.000000000000000000, 0.000000000000000000, 0.000000000000000000 ) ) ;
#19469 = CARTESIAN_POINT ( 'NONE',  ( 0.000000000000000000, 0.000000000000000000, 0.000000000000000000 ) ) ;
#19470 = EDGE_LOOP ( 'NONE', ( #4714, #1450, #1098, #11061 ) ) ;
#19471 = ORIENTED_EDGE ( 'NONE', *, *, #21065, .T. ) ;
#19472 = CARTESIAN_POINT ( 'NONE',  ( 0.000000000000000000, 25.48117629651189375, 10.33947075754270095 ) ) ;
#19473 = DIRECTION ( 'NONE',  ( -1.000000000000000000, -0.000000000000000000, 0.000000000000000000 ) ) ;
#19474 = DIRECTION ( 'NONE',  ( 0.000000000000000000, 0.000000000000000000, 1.000000000000000000 ) ) ;
#19475 = ADVANCED_FACE ( 'NONE', ( #16284 ), #14631, .T. ) ;
#19476 = FACE_BOUND ( 'NONE', #4949, .T. ) ;
#19477 = CARTESIAN_POINT ( 'NONE',  ( 5.000000000000000000, 41.89587599971653731, -77.38692120905427885 ) ) ;
#19478 = DIRECTION ( 'NONE',  ( -1.000000000000000000, 0.000000000000000000, 0.000000000000000000 ) ) ;
#19479 = CARTESIAN_POINT ( 'NONE',  ( 10.00000000000000000, 71.72924546249947753, 45.71766382684695884 ) ) ;
#19480 = CARTESIAN_POINT ( 'NONE',  ( 10.00000000000000000, 75.45728100697654384, -39.26051685138985903 ) ) ;
#19481 = LINE ( 'NONE', #16055, #16886 ) ;
#19482 = DIRECTION ( 'NONE',  ( 0.000000000000000000, 0.000000000000000000, 1.000000000000000000 ) ) ;
#19483 = AXIS2_PLACEMENT_3D ( 'NONE', #20707, #16014, #21434 ) ;
#19484 = VERTEX_POINT ( 'NONE', #19493 ) ;
#19485 = CARTESIAN_POINT ( 'NONE',  ( 10.00000000000000000, 48.19312842678472464, 70.09002648625214249 ) ) ;
#19486 = EDGE_CURVE ( 'NONE', #5395, #15764, #14084, .T. ) ;
#19487 = ORIENTED_EDGE ( 'NONE', *, *, #8082, .F. ) ;
#19488 = EDGE_CURVE ( 'NONE', #1594, #8339, #4564, .T. ) ;
#19489 = CARTESIAN_POINT ( 'NONE',  ( 10.00000000000000000, -2.208823992043557283, -85.03123271466938604 ) ) ;
#19490 = FACE_OUTER_BOUND ( 'NONE', #9788, .T. ) ;
#19491 = AXIS2_PLACEMENT_3D ( 'NONE', #10396, #7318, #12484 ) ;
#19492 = EDGE_CURVE ( 'NONE', #4876, #2112, #1154, .T. ) ;
#19493 = CARTESIAN_POINT ( 'NONE',  ( 10.00000000000000000, -51.18896083639317851, 71.57995730992162464 ) ) ;
#19494 = ORIENTED_EDGE ( 'NONE', *, *, #5031, .T. ) ;
#19495 = ADVANCED_FACE ( 'NONE', ( #723 ), #4358, .T. ) ;
#19496 = PRESENTATION_STYLE_ASSIGNMENT (( #17964 ) ) ;
#19497 = EDGE_LOOP ( 'NONE', ( #9763, #18824, #16981, #12849 ) ) ;
#19498 = ORIENTED_EDGE ( 'NONE', *, *, #6496, .T. ) ;
#19499 = ORIENTED_EDGE ( 'NONE', *, *, #7365, .T. ) ;
#19500 = DIRECTION ( 'NONE',  ( 0.000000000000000000, -0.4694715627858798146, -0.8829475928589327616 ) ) ;
#19501 = DIRECTION ( 'NONE',  ( 0.000000000000000000, 0.9945218953682729568, 0.1045284632676570791 ) ) ;
#19502 = CIRCLE ( 'NONE', #11375, 3.000000000000000444 ) ;
#19503 = EDGE_LOOP ( 'NONE', ( #17356, #5004, #15989, #377 ) ) ;
#19504 = CARTESIAN_POINT ( 'NONE',  ( 0.000000000000000000, -19.07277123396555041, 19.80970465344741882 ) ) ;
#19505 = DIRECTION ( 'NONE',  ( -1.000000000000000000, 0.000000000000000000, -0.000000000000000000 ) ) ;
#19506 = DIRECTION ( 'NONE',  ( 0.000000000000000000, 0.000000000000000000, -1.000000000000000000 ) ) ;
#19507 = DIRECTION ( 'NONE',  ( -1.000000000000000000, -0.000000000000000000, -0.000000000000000000 ) ) ;
#19508 = LINE ( 'NONE', #7911, #10892 ) ;
#19509 = AXIS2_PLACEMENT_3D ( 'NONE', #5518, #12248, #14127 ) ;
#19510 = ORIENTED_EDGE ( 'NONE', *, *, #18884, .T. ) ;
#19511 = CARTESIAN_POINT ( 'NONE',  ( 0.000000000000000000, -7.619321854369744074, 26.42235673590688094 ) ) ;
#19512 = CIRCLE ( 'NONE', #17045, 11.99999999999999822 ) ;
#19513 = FACE_OUTER_BOUND ( 'NONE', #18913, .T. ) ;
#19514 = AXIS2_PLACEMENT_3D ( 'NONE', #7012, #10742, #20703 ) ;
#19515 = CARTESIAN_POINT ( 'NONE',  ( 0.000000000000000000, 0.000000000000000000, 0.000000000000000000 ) ) ;
#19516 = VERTEX_POINT ( 'NONE', #21264 ) ;
#19517 = DIRECTION ( 'NONE',  ( 0.000000000000000000, 0.000000000000000000, -1.000000000000000000 ) ) ;
#19518 = ORIENTED_EDGE ( 'NONE', *, *, #588, .T. ) ;
#19519 = CARTESIAN_POINT ( 'NONE',  ( 5.000000000000002665, -12.90135963484139658, 87.04915231966639055 ) ) ;
#19520 = EDGE_LOOP ( 'NONE', ( #21571, #18471, #237, #20209 ) ) ;
#19521 = DIRECTION ( 'NONE',  ( -1.000000000000000000, 0.000000000000000000, -0.000000000000000000 ) ) ;
#19522 = AXIS2_PLACEMENT_3D ( 'NONE', #21416, #11022, #2520 ) ;
#19523 = ORIENTED_EDGE ( 'NONE', *, *, #17662, .T. ) ;
#19524 = ORIENTED_EDGE ( 'NONE', *, *, #372, .F. ) ;
#19525 = CARTESIAN_POINT ( 'NONE',  ( 10.00000000000000000, -16.79755869217711250, 90.96305306542248559 ) ) ;
#19526 = VERTEX_POINT ( 'NONE', #5914 ) ;
#19527 = CYLINDRICAL_SURFACE ( 'NONE', #3488, 45.00000000000000000 ) ;
#19528 = AXIS2_PLACEMENT_3D ( 'NONE', #3049, #2931, #9891 ) ;
#19529 = DIRECTION ( 'NONE',  ( 1.000000000000000000, 0.000000000000000000, 0.000000000000000000 ) ) ;
#19530 = DIRECTION ( 'NONE',  ( 0.000000000000000000, 0.000000000000000000, 1.000000000000000000 ) ) ;
#19531 = LINE ( 'NONE', #17893, #1877 ) ;
#19532 = AXIS2_PLACEMENT_3D ( 'NONE', #13443, #8802, #402 ) ;
#19533 = AXIS2_PLACEMENT_3D ( 'NONE', #5111, #13725, #20365 ) ;
#19534 = DIRECTION ( 'NONE',  ( 0.000000000000000000, 0.000000000000000000, -1.000000000000000000 ) ) ;
#19535 = DIRECTION ( 'NONE',  ( 1.000000000000000000, 0.000000000000000000, 0.000000000000000000 ) ) ;
#19536 = DIRECTION ( 'NONE',  ( 0.000000000000000000, 0.000000000000000000, -1.000000000000000000 ) ) ;
#19537 = CARTESIAN_POINT ( 'NONE',  ( 0.000000000000000000, 0.000000000000000000, 0.000000000000000000 ) ) ;
#19538 = CIRCLE ( 'NONE', #7906, 45.00000000000000711 ) ;
#19539 = DIRECTION ( 'NONE',  ( 0.000000000000000000, 0.000000000000000000, 1.000000000000000000 ) ) ;
#19540 = AXIS2_PLACEMENT_3D ( 'NONE', #16945, #6782, #1691 ) ;
#19541 = EDGE_LOOP ( 'NONE', ( #19069, #1790, #5427, #12700 ) ) ;
#19542 = EDGE_CURVE ( 'NONE', #13591, #11791, #17279, .T. ) ;
#19543 = VERTEX_POINT ( 'NONE', #19280 ) ;
#19544 = CIRCLE ( 'NONE', #10728, 5.000000000000000000 ) ;
#19545 = ORIENTED_EDGE ( 'NONE', *, *, #10560, .T. ) ;
#19546 = ORIENTED_EDGE ( 'NONE', *, *, #17717, .F. ) ;
#19547 = ADVANCED_FACE ( 'NONE', ( #17847 ), #4255, .F. ) ;
#19548 = ORIENTED_EDGE ( 'NONE', *, *, #1112, .F. ) ;
#19549 = FACE_OUTER_BOUND ( 'NONE', #15885, .T. ) ;
#19550 = VECTOR ( 'NONE', #15735, 1000.000000000000000 ) ;
#19551 = ORIENTED_EDGE ( 'NONE', *, *, #9486, .T. ) ;
#19552 = LINE ( 'NONE', #12304, #20550 ) ;
#19553 = DIRECTION ( 'NONE',  ( -1.000000000000000000, -0.000000000000000000, 0.000000000000000000 ) ) ;
#19554 = CARTESIAN_POINT ( 'NONE',  ( 10.00000000000000000, 0.000000000000000000, 0.000000000000000000 ) ) ;
#19555 = AXIS2_PLACEMENT_3D ( 'NONE', #5057, #2069, #3399 ) ;
#19556 = CARTESIAN_POINT ( 'NONE',  ( 0.000000000000000000, -14.53731623274912366, -23.34226719384920656 ) ) ;
#19557 = LINE ( 'NONE', #9499, #1364 ) ;
#19558 = CARTESIAN_POINT ( 'NONE',  ( -2.799999999999996714, 60.00000000000000000, -15.00000000000000000 ) ) ;
#19559 = CIRCLE ( 'NONE', #5108, 11.99999999999999822 ) ;
#19560 = FACE_OUTER_BOUND ( 'NONE', #19311, .T. ) ;
#19561 = DIRECTION ( 'NONE',  ( -1.000000000000000000, 0.000000000000000000, -0.000000000000000000 ) ) ;
#19562 = CARTESIAN_POINT ( 'NONE',  ( 10.00000000000000000, 0.000000000000000000, 0.000000000000000000 ) ) ;
#19563 = ORIENTED_EDGE ( 'NONE', *, *, #18790, .T. ) ;
#19564 = CARTESIAN_POINT ( 'NONE',  ( 0.000000000000000000, 51.18896083639367589, -71.57995730992126937 ) ) ;
#19565 = VECTOR ( 'NONE', #2197, 1000.000000000000000 ) ;
#19566 = EDGE_CURVE ( 'NONE', #15663, #9924, #17736, .T. ) ;
#19568 = ADVANCED_FACE ( 'NONE', ( #9317 ), #12859, .T. ) ;
#19567 = CONICAL_SURFACE ( 'NONE', #10044, 5.453125000000000000, 0.4883339510564123076 ) ;
#19569 = EDGE_CURVE ( 'NONE', #2662, #733, #10910, .T. ) ;
#19570 = VERTEX_POINT ( 'NONE', #21164 ) ;
#19571 = CIRCLE ( 'NONE', #6584, 88.00000000000000000 ) ;
#19572 = CARTESIAN_POINT ( 'NONE',  ( 5.000000000000000888, -7.240962358591787940, 31.16999300804312156 ) ) ;
#19574 = AXIS2_PLACEMENT_3D ( 'NONE', #13731, #3668, #20478 ) ;
#19573 = AXIS2_PLACEMENT_3D ( 'NONE', #4129, #17619, #15941 ) ;
#19575 = ADVANCED_FACE ( 'NONE', ( #6034 ), #7790, .F. ) ;
#19576 = DIRECTION ( 'NONE',  ( 0.000000000000000000, 0.000000000000000000, 1.000000000000000000 ) ) ;
#19577 = ORIENTED_EDGE ( 'NONE', *, *, #18562, .F. ) ;
#19578 = CARTESIAN_POINT ( 'NONE',  ( 0.000000000000000000, 29.47587714451147534, -82.91666097089093057 ) ) ;
#19579 = ORIENTED_EDGE ( 'NONE', *, *, #1097, .T. ) ;
#19580 = ORIENTED_EDGE ( 'NONE', *, *, #6381, .F. ) ;
#19581 = CIRCLE ( 'NONE', #3348, 44.99999999999998579 ) ;
#19582 = PRODUCT_CONTEXT ( 'NONE', #16715, 'mechanical' ) ;
#19583 = DIRECTION ( 'NONE',  ( 1.000000000000000000, 0.000000000000000000, 0.000000000000000000 ) ) ;
#19584 = ORIENTED_EDGE ( 'NONE', *, *, #7582, .F. ) ;
#19585 = VERTEX_POINT ( 'NONE', #17636 ) ;
#19586 = DIRECTION ( 'NONE',  ( 0.000000000000000000, 0.8290375725550390706, 0.5591929034707506796 ) ) ;
#19587 = DIRECTION ( 'NONE',  ( 0.000000000000000000, 0.000000000000000000, 1.000000000000000000 ) ) ;
#19588 = EDGE_CURVE ( 'NONE', #4269, #15626, #13739, .T. ) ;
#19589 = DIRECTION ( 'NONE',  ( 0.000000000000000000, 0.000000000000000000, 1.000000000000000000 ) ) ;
#19590 = DIRECTION ( 'NONE',  ( 0.000000000000000000, 0.000000000000000000, 1.000000000000000000 ) ) ;
#19591 = AXIS2_PLACEMENT_3D ( 'NONE', #10869, #7783, #17624 ) ;
#19592 = AXIS2_PLACEMENT_3D ( 'NONE', #17429, #15766, #12664 ) ;
#19593 = DIRECTION ( 'NONE',  ( 0.000000000000000000, 0.000000000000000000, -1.000000000000000000 ) ) ;
#19594 = VECTOR ( 'NONE', #9973, 1000.000000000000000 ) ;
#19595 = FACE_OUTER_BOUND ( 'NONE', #3119, .T. ) ;
#19596 = AXIS2_PLACEMENT_3D ( 'NONE', #8135, #3155, #11665 ) ;
#19597 = DIRECTION ( 'NONE',  ( 0.000000000000000000, 2.127927463864883580E-14, -1.000000000000000000 ) ) ;
#19598 = EDGE_CURVE ( 'NONE', #3682, #12932, #8450, .T. ) ;
#19599 = CARTESIAN_POINT ( 'NONE',  ( 10.00000000000000000, -92.22057093985034726, 7.197311757040196767 ) ) ;
#19601 = AXIS2_PLACEMENT_3D ( 'NONE', #21680, #3337, #11846 ) ;
#19600 = CYLINDRICAL_SURFACE ( 'NONE', #15076, 88.00000000000000000 ) ;
#19602 = ORIENTED_EDGE ( 'NONE', *, *, #937, .T. ) ;
#19603 = DIRECTION ( 'NONE',  ( -1.000000000000000000, 0.000000000000000000, 0.000000000000000000 ) ) ;
#19604 = ORIENTED_EDGE ( 'NONE', *, *, #12063, .F. ) ;
#19605 = EDGE_CURVE ( 'NONE', #21544, #12774, #12969, .T. ) ;
#19606 = DIRECTION ( 'NONE',  ( 0.000000000000000000, -1.954455116267202870E-14, -1.000000000000000000 ) ) ;
#19607 = EDGE_CURVE ( 'NONE', #9814, #14447, #18347, .T. ) ;
#19608 = CIRCLE ( 'NONE', #1269, 32.00000000000000000 ) ;
#19609 = DIRECTION ( 'NONE',  ( 0.000000000000000000, 0.000000000000000000, 1.000000000000000000 ) ) ;
#19610 = ORIENTED_EDGE ( 'NONE', *, *, #128, .F. ) ;
#19611 = CIRCLE ( 'NONE', #10077, 88.00000000000000000 ) ;
#19612 = VECTOR ( 'NONE', #12928, 1000.000000000000000 ) ;
#19613 = VERTEX_POINT ( 'NONE', #4584 ) ;
#19614 = VERTEX_POINT ( 'NONE', #1476 ) ;
#19615 = ORIENTED_EDGE ( 'NONE', *, *, #3520, .T. ) ;
#19616 = DIRECTION ( 'NONE',  ( 0.000000000000000000, 0.9848077530122074652, 0.1736481776669340227 ) ) ;
#19617 = CYLINDRICAL_SURFACE ( 'NONE', #4860, 9.999999999999998224 ) ;
#19618 = ORIENTED_EDGE ( 'NONE', *, *, #8911, .F. ) ;
#19619 = EDGE_CURVE ( 'NONE', #2060, #2977, #19820, .T. ) ;
#19620 = FACE_OUTER_BOUND ( 'NONE', #7860, .T. ) ;
#19621 = DIRECTION ( 'NONE',  ( 0.000000000000000000, 0.000000000000000000, -1.000000000000000000 ) ) ;
#19622 = DIRECTION ( 'NONE',  ( -1.000000000000000000, -0.000000000000000000, 0.000000000000000000 ) ) ;
#19623 = ADVANCED_FACE ( 'NONE', ( #19931, #11422 ), #13298, .T. ) ;
#19624 = DIRECTION ( 'NONE',  ( -1.000000000000000000, 0.000000000000000000, 0.000000000000000000 ) ) ;
#19625 = LINE ( 'NONE', #6272, #8079 ) ;
#19626 = AXIS2_PLACEMENT_3D ( 'NONE', #11620, #18367, #10172 ) ;
#19627 = EDGE_CURVE ( 'NONE', #4382, #16727, #8304, .T. ) ;
#19628 = ORIENTED_EDGE ( 'NONE', *, *, #7582, .T. ) ;
#19629 = CIRCLE ( 'NONE', #12569, 88.00000000000000000 ) ;
#19630 = EDGE_CURVE ( 'NONE', #2742, #5097, #5498, .T. ) ;
#19631 = DIRECTION ( 'NONE',  ( -1.000000000000000000, -0.000000000000000000, -0.000000000000000000 ) ) ;
#19632 = CONICAL_SURFACE ( 'NONE', #7941, 104.9000000000000341, 0.5675376247847546685 ) ;
#19633 = FACE_OUTER_BOUND ( 'NONE', #5446, .T. ) ;
#19634 = ORIENTED_EDGE ( 'NONE', *, *, #5671, .T. ) ;
#19635 = CARTESIAN_POINT ( 'NONE',  ( 0.000000000000000000, -1.959304526717615902, -27.42911093658677402 ) ) ;
#19636 = ORIENTED_EDGE ( 'NONE', *, *, #2485, .F. ) ;
#19637 = EDGE_CURVE ( 'NONE', #15746, #20991, #5851, .T. ) ;
#19638 = CARTESIAN_POINT ( 'NONE',  ( 9.999999999999994671, 0.000000000000000000, 0.000000000000000000 ) ) ;
#19639 = CARTESIAN_POINT ( 'NONE',  ( 0.000000000000000000, 0.000000000000000000, 0.000000000000000000 ) ) ;
#19640 = ORIENTED_EDGE ( 'NONE', *, *, #3110, .T. ) ;
#19641 = DIRECTION ( 'NONE',  ( -1.000000000000000000, 0.000000000000000000, -0.000000000000000000 ) ) ;
#19642 = ORIENTED_EDGE ( 'NONE', *, *, #10180, .F. ) ;
#19643 = AXIS2_PLACEMENT_3D ( 'NONE', #6310, #11150, #12791 ) ;
#19644 = EDGE_LOOP ( 'NONE', ( #12672, #6933, #4263, #14517 ) ) ;
#19645 = DIRECTION ( 'NONE',  ( 1.000000000000000000, 0.000000000000000000, 0.000000000000000000 ) ) ;
#19646 = AXIS2_PLACEMENT_3D ( 'NONE', #14047, #14487, #16021 ) ;
#19647 = VERTEX_POINT ( 'NONE', #6255 ) ;
#19648 = CARTESIAN_POINT ( 'NONE',  ( 10.00000000000000000, 0.000000000000000000, 0.000000000000000000 ) ) ;
#19649 = LINE ( 'NONE', #21531, #13219 ) ;
#19650 = CARTESIAN_POINT ( 'NONE',  ( 10.00000000000000000, 0.000000000000000000, 0.000000000000000000 ) ) ;
#19651 = FACE_OUTER_BOUND ( 'NONE', #17385, .T. ) ;
#19652 = FACE_OUTER_BOUND ( 'NONE', #8147, .T. ) ;
#19653 = DIRECTION ( 'NONE',  ( 1.000000000000000000, 0.000000000000000000, 0.000000000000000000 ) ) ;
#19654 = ADVANCED_FACE ( 'NONE', ( #3141 ), #3033, .F. ) ;
#19655 = DIRECTION ( 'NONE',  ( 0.000000000000000000, 0.000000000000000000, 1.000000000000000000 ) ) ;
#19656 = FACE_OUTER_BOUND ( 'NONE', #8065, .T. ) ;
#19657 = AXIS2_PLACEMENT_3D ( 'NONE', #8732, #15349, #18898 ) ;
#19658 = AXIS2_PLACEMENT_3D ( 'NONE', #21832, #2942, #13206 ) ;
#19659 = CARTESIAN_POINT ( 'NONE',  ( 0.000000000000000000, 0.000000000000000000, -3.000000000000000000 ) ) ;
#19660 = ORIENTED_EDGE ( 'NONE', *, *, #5342, .T. ) ;
#19661 = ORIENTED_EDGE ( 'NONE', *, *, #6425, .F. ) ;
#19662 = VERTEX_POINT ( 'NONE', #5013 ) ;
#19663 = VERTEX_POINT ( 'NONE', #20157 ) ;
#19664 = VERTEX_POINT ( 'NONE', #16719 ) ;
#19665 = DIRECTION ( 'NONE',  ( 0.000000000000000000, 0.000000000000000000, 1.000000000000000000 ) ) ;
#19666 = AXIS2_PLACEMENT_3D ( 'NONE', #1429, #11473, #11148 ) ;
#19667 = ORIENTED_EDGE ( 'NONE', *, *, #8507, .T. ) ;
#19668 = LINE ( 'NONE', #7632, #17374 ) ;
#19669 = VECTOR ( 'NONE', #2810, 1000.000000000000000 ) ;
#19670 = DIRECTION ( 'NONE',  ( -1.000000000000000000, 0.000000000000000000, -0.000000000000000000 ) ) ;
#19671 = CARTESIAN_POINT ( 'NONE',  ( -90.00000000000000000, 0.000000000000000000, 0.000000000000000000 ) ) ;
#19672 = CARTESIAN_POINT ( 'NONE',  ( 2.000000000000000000, 70.00000000000000000, 9.999999999999998224 ) ) ;
#19673 = EDGE_CURVE ( 'NONE', #8121, #6764, #1271, .T. ) ;
#19674 = CARTESIAN_POINT ( 'NONE',  ( 0.000000000000000000, 0.000000000000000000, 0.000000000000000000 ) ) ;
#19675 = CARTESIAN_POINT ( 'NONE',  ( 5.000000000000002665, -35.18804927320584142, 80.65854690202667143 ) ) ;
#19676 = FACE_OUTER_BOUND ( 'NONE', #13157, .T. ) ;
#19677 = VERTEX_POINT ( 'NONE', #18398 ) ;
#19678 = PRODUCT_DEFINITION ( 'UNKNOWN', '', #17697, #8727 ) ;
#19679 = DIRECTION ( 'NONE',  ( -1.000000000000000000, 0.000000000000000000, 0.000000000000000000 ) ) ;
#19680 = AXIS2_PLACEMENT_3D ( 'NONE', #457, #10719, #5433 ) ;
#19681 = AXIS2_PLACEMENT_3D ( 'NONE', #15544, #14104, #17094 ) ;
#19682 = ORIENTED_EDGE ( 'NONE', *, *, #13738, .T. ) ;
#19683 = CIRCLE ( 'NONE', #3463, 92.50100000000000477 ) ;
#19684 = DIRECTION ( 'NONE',  ( 1.000000000000000000, -0.000000000000000000, -0.000000000000000000 ) ) ;
#19685 = CARTESIAN_POINT ( 'NONE',  ( -10.00000000000000000, 0.000000000000000000, 0.000000000000000000 ) ) ;
#19686 = VERTEX_POINT ( 'NONE', #9758 ) ;
#19687 = CARTESIAN_POINT ( 'NONE',  ( 10.00000000000000000, -32.56745702629792305, 78.57830605990643846 ) ) ;
#19688 = ORIENTED_EDGE ( 'NONE', *, *, #15811, .T. ) ;
#19689 = ORIENTED_EDGE ( 'NONE', *, *, #9488, .F. ) ;
#19690 = APPLICATION_PROTOCOL_DEFINITION ( 'draft international standard', 'automotive_design', 1998, #11362 ) ;
#19691 = VECTOR ( 'NONE', #5992, 1000.000000000000000 ) ;
#19692 = APPLICATION_CONTEXT ( 'automotive_design' ) ;
#19693 = CYLINDRICAL_SURFACE ( 'NONE', #5079, 45.00000000000000000 ) ;
#19694 = VERTEX_POINT ( 'NONE', #1588 ) ;
#19695 = ORIENTED_EDGE ( 'NONE', *, *, #21745, .T. ) ;
#19696 = CARTESIAN_POINT ( 'NONE',  ( 10.00000000000000000, 52.25832601289098278, 70.80301803122803506 ) ) ;
#19697 = CARTESIAN_POINT ( 'NONE',  ( 0.000000000000000000, 0.000000000000000000, 0.000000000000000000 ) ) ;
#19698 = AXIS2_PLACEMENT_3D ( 'NONE', #674, #7418, #17032 ) ;
#19699 = CARTESIAN_POINT ( 'NONE',  ( 10.00000000000000000, -7.240962358591358061, -31.16999300804321749 ) ) ;
#19700 = DIRECTION ( 'NONE',  ( 0.000000000000000000, 0.7431448254773910245, 0.6691306063588617903 ) ) ;
#19701 = EDGE_CURVE ( 'NONE', #9457, #18200, #3242, .T. ) ;
#19702 = CIRCLE ( 'NONE', #3838, 92.50100000000000477 ) ;
#19703 = DIRECTION ( 'NONE',  ( 1.000000000000000000, 0.000000000000000000, 0.000000000000000000 ) ) ;
#19704 = AXIS2_PLACEMENT_3D ( 'NONE', #4661, #16264, #1126 ) ;
#19705 = FACE_OUTER_BOUND ( 'NONE', #959, .T. ) ;
#19706 = AXIS2_PLACEMENT_3D ( 'NONE', #7642, #5768, #15923 ) ;
#19707 = CARTESIAN_POINT ( 'NONE',  ( -8.000000000000007105, 0.000000000000000000, -104.9000000000000341 ) ) ;
#19708 = CYLINDRICAL_SURFACE ( 'NONE', #11485, 44.99999999999998579 ) ;
#19709 = CARTESIAN_POINT ( 'NONE',  ( 0.000000000000000000, -86.54587337002867287, -15.93147207947093946 ) ) ;
#19710 = VERTEX_POINT ( 'NONE', #21587 ) ;
#19711 = VERTEX_POINT ( 'NONE', #10088 ) ;
#19712 = CARTESIAN_POINT ( 'NONE',  ( 10.00000000000000000, -6.063030049135288202, 31.42037024962122871 ) ) ;
#19713 = EDGE_CURVE ( 'NONE', #6864, #7736, #20665, .T. ) ;
#19714 = AXIS2_PLACEMENT_3D ( 'NONE', #13693, #1983, #5630 ) ;
#19715 = DIRECTION ( 'NONE',  ( 0.000000000000000000, -0.4067366430757888285, -0.9135454576426059736 ) ) ;
#19716 = AXIS2_PLACEMENT_3D ( 'NONE', #19848, #4713, #6609 ) ;
#19717 = MECHANICAL_DESIGN_GEOMETRIC_PRESENTATION_REPRESENTATION (  '', ( #21830 ), #10193 ) ;
#19718 = DIRECTION ( 'NONE',  ( -0.000000000000000000, -0.000000000000000000, -1.000000000000000000 ) ) ;
#19719 = CIRCLE ( 'NONE', #13357, 44.99999999999999289 ) ;
#19720 = VERTEX_POINT ( 'NONE', #11750 ) ;
#19721 = ORIENTED_EDGE ( 'NONE', *, *, #8132, .T. ) ;
#19722 = ORIENTED_EDGE ( 'NONE', *, *, #2867, .F. ) ;
#19723 = EDGE_LOOP ( 'NONE', ( #15242, #11340, #9436, #17008 ) ) ;
#19724 = FACE_OUTER_BOUND ( 'NONE', #15084, .T. ) ;
#19725 = CYLINDRICAL_SURFACE ( 'NONE', #13951, 88.00000000000000000 ) ;
#19726 = EDGE_LOOP ( 'NONE', ( #2352, #18909, #67, #4420 ) ) ;
#19727 = EDGE_CURVE ( 'NONE', #6116, #2973, #6368, .T. ) ;
#19728 = FACE_OUTER_BOUND ( 'NONE', #1977, .T. ) ;
#19729 = CARTESIAN_POINT ( 'NONE',  ( 0.000000000000000000, 0.000000000000000000, 0.000000000000000000 ) ) ;
#19730 = EDGE_CURVE ( 'NONE', #8068, #286, #6581, .T. ) ;
#19731 = CYLINDRICAL_SURFACE ( 'NONE', #17140, 88.00000000000000000 ) ;
#19732 = EDGE_CURVE ( 'NONE', #5370, #13890, #11487, .T. ) ;
#19733 = DIRECTION ( 'NONE',  ( 1.000000000000000000, 0.000000000000000000, 0.000000000000000000 ) ) ;
#19734 = DIRECTION ( 'NONE',  ( 1.000000000000000000, 0.000000000000000000, 0.000000000000000000 ) ) ;
#19735 = AXIS2_PLACEMENT_3D ( 'NONE', #10014, #1632, #21530 ) ;
#19736 = EDGE_CURVE ( 'NONE', #12830, #18956, #6196, .T. ) ;
#19737 = AXIS2_PLACEMENT_3D ( 'NONE', #9423, #20935, #12749 ) ;
#19738 =( GEOMETRIC_REPRESENTATION_CONTEXT ( 3 ) GLOBAL_UNCERTAINTY_ASSIGNED_CONTEXT ( ( #6386 ) ) GLOBAL_UNIT_ASSIGNED_CONTEXT ( ( #11681, #1943, #8358 ) ) REPRESENTATION_CONTEXT ( 'NONE', 'WORKASPACE' ) );
#19739 = ORIENTED_EDGE ( 'NONE', *, *, #6813, .T. ) ;
#19740 = AXIS2_PLACEMENT_3D ( 'NONE', #5389, #6627, #3516 ) ;
#19741 = DIRECTION ( 'NONE',  ( 0.000000000000000000, -0.2079116908177664202, 0.9781476007338040235 ) ) ;
#19742 = ADVANCED_FACE ( 'NONE', ( #19042 ), #20586, .F. ) ;
#19743 = DIRECTION ( 'NONE',  ( 0.000000000000000000, -0.8987940462991710344, 0.4383711467890689106 ) ) ;
#19744 = ORIENTED_EDGE ( 'NONE', *, *, #17699, .T. ) ;
#19745 = CARTESIAN_POINT ( 'NONE',  ( -10.00000000000000000, 0.000000000000000000, 0.000000000000000000 ) ) ;
#19746 = EDGE_CURVE ( 'NONE', #8452, #11211, #477, .T. ) ;
#19747 = EDGE_LOOP ( 'NONE', ( #9049, #19642 ) ) ;
#19748 = CARTESIAN_POINT ( 'NONE',  ( 0.000000000000000000, 0.000000000000000000, 0.000000000000000000 ) ) ;
#19749 = LINE ( 'NONE', #14443, #5958 ) ;
#19750 = ORIENTED_EDGE ( 'NONE', *, *, #10648, .F. ) ;
#19751 = CARTESIAN_POINT ( 'NONE',  ( 10.00000000000000000, -75.87763420127802760, -44.57111876559801544 ) ) ;
#19752 = EDGE_CURVE ( 'NONE', #21211, #14549, #14300, .T. ) ;
#19753 = VECTOR ( 'NONE', #7777, 1000.000000000000000 ) ;
#19754 = VERTEX_POINT ( 'NONE', #8865 ) ;
#19755 = ORIENTED_EDGE ( 'NONE', *, *, #16912, .T. ) ;
#19756 = DIRECTION ( 'NONE',  ( -1.000000000000000000, 0.000000000000000000, -0.000000000000000000 ) ) ;
#19757 = CIRCLE ( 'NONE', #10928, 44.99999999999999289 ) ;
#19758 = EDGE_CURVE ( 'NONE', #4982, #17286, #11832, .T. ) ;
#19759 = ORIENTED_EDGE ( 'NONE', *, *, #1379, .F. ) ;
#19760 = DIRECTION ( 'NONE',  ( 0.000000000000000000, -9.251858538542973800E-16, -1.000000000000000000 ) ) ;
#19761 = CARTESIAN_POINT ( 'NONE',  ( 10.00000000000000000, 91.70173545986537533, -12.13370160539944287 ) ) ;
#19762 = CARTESIAN_POINT ( 'NONE',  ( -10.00000000000000000, 0.000000000000000000, 0.000000000000000000 ) ) ;
#19763 = DIRECTION ( 'NONE',  ( 0.000000000000000000, -0.7431448254773862505, -0.6691306063588668973 ) ) ;
#19764 = ADVANCED_FACE ( 'NONE', ( #10523 ), #2026, .F. ) ;
#19765 = FACE_OUTER_BOUND ( 'NONE', #16309, .T. ) ;
#19766 = DIRECTION ( 'NONE',  ( 0.000000000000000000, 0.000000000000000000, 1.000000000000000000 ) ) ;
#19767 = DIRECTION ( 'NONE',  ( 0.000000000000000000, 0.2756373558169997184, -0.9612616959383185611 ) ) ;
#19768 = CARTESIAN_POINT ( 'NONE',  ( 10.00000000000000000, -21.31452625070873452, -82.34610137166143318 ) ) ;
#19769 = CYLINDRICAL_SURFACE ( 'NONE', #8642, 44.99999999999999289 ) ;
#19770 = AXIS2_PLACEMENT_3D ( 'NONE', #19685, #17602, #11064 ) ;
#19771 = FACE_OUTER_BOUND ( 'NONE', #300, .T. ) ;
#19772 = ORIENTED_EDGE ( 'NONE', *, *, #14887, .F. ) ;
#19773 = VERTEX_POINT ( 'NONE', #20378 ) ;
#19774 = EDGE_CURVE ( 'NONE', #7680, #3874, #15017, .T. ) ;
#19775 = EDGE_LOOP ( 'NONE', ( #19158, #3333, #9910, #13179 ) ) ;
#19776 = ORIENTED_EDGE ( 'NONE', *, *, #5550, .F. ) ;
#19777 = ADVANCED_FACE ( 'NONE', ( #6792 ), #10303, .F. ) ;
#19778 = EDGE_CURVE ( 'NONE', #5510, #5864, #16422, .T. ) ;
#19779 = EDGE_LOOP ( 'NONE', ( #17194, #7950, #5132, #15561 ) ) ;
#19780 = FACE_OUTER_BOUND ( 'NONE', #20562, .T. ) ;
#19781 = VERTEX_POINT ( 'NONE', #5238 ) ;
#19782 = CARTESIAN_POINT ( 'NONE',  ( -10.00000000000000000, 0.000000000000000000, 0.000000000000000000 ) ) ;
#19783 = AXIS2_PLACEMENT_3D ( 'NONE', #8624, #7192, #20670 ) ;
#19784 = DIRECTION ( 'NONE',  ( -1.000000000000000000, 0.000000000000000000, -0.000000000000000000 ) ) ;
#19785 = CYLINDRICAL_SURFACE ( 'NONE', #11491, 6.728125000000023448 ) ;
#19786 = DIRECTION ( 'NONE',  ( -1.000000000000000000, 0.000000000000000000, 0.000000000000000000 ) ) ;
#19787 = CARTESIAN_POINT ( 'NONE',  ( 10.00000000000000000, -17.64925110578410639, -86.21197095186363413 ) ) ;
#19788 = LINE ( 'NONE', #13145, #6612 ) ;
#19789 = CARTESIAN_POINT ( 'NONE',  ( 10.00000000000000000, 0.000000000000000000, 0.000000000000000000 ) ) ;
#19790 = CIRCLE ( 'NONE', #12729, 120.0000000000000284 ) ;
#19791 = ORIENTED_EDGE ( 'NONE', *, *, #11613, .T. ) ;
#19792 = CARTESIAN_POINT ( 'NONE',  ( 7.999999999999979572, 1.409568465818603827E-14, 115.1000000000000227 ) ) ;
#19793 =( GEOMETRIC_REPRESENTATION_CONTEXT ( 3 ) GLOBAL_UNCERTAINTY_ASSIGNED_CONTEXT ( ( #4601 ) ) GLOBAL_UNIT_ASSIGNED_CONTEXT ( ( #13982, #18964, #14302 ) ) REPRESENTATION_CONTEXT ( 'NONE', 'WORKASPACE' ) );
#19794 = ORIENTED_EDGE ( 'NONE', *, *, #1221, .F. ) ;
#19795 = ORIENTED_EDGE ( 'NONE', *, *, #6042, .F. ) ;
#19796 = CARTESIAN_POINT ( 'NONE',  ( 0.000000000000000000, -56.05743251323810483, -67.83483072893858434 ) ) ;
#19797 = DIRECTION ( 'NONE',  ( 0.000000000000000000, -0.9702957262759988044, 0.2419218955996582376 ) ) ;
#19798 = ORIENTED_EDGE ( 'NONE', *, *, #21697, .F. ) ;
#19799 = LINE ( 'NONE', #1351, #5959 ) ;
#19800 = EDGE_LOOP ( 'NONE', ( #4710, #8549, #5320, #2643 ) ) ;
#19801 = EDGE_LOOP ( 'NONE', ( #2641, #20827, #18299, #20214 ) ) ;
#19802 = VECTOR ( 'NONE', #19561, 1000.000000000000000 ) ;
#19803 = DIRECTION ( 'NONE',  ( 1.000000000000000000, 0.000000000000000000, 0.000000000000000000 ) ) ;
#19804 = CARTESIAN_POINT ( 'NONE',  ( 10.00000000000000000, 0.000000000000000000, 0.000000000000000000 ) ) ;
#19805 = ORIENTED_EDGE ( 'NONE', *, *, #12048, .F. ) ;
#19806 = CARTESIAN_POINT ( 'NONE',  ( -1.200000000000006617, 0.000000000000000000, 0.000000000000000000 ) ) ;
#19807 = DIRECTION ( 'NONE',  ( 0.000000000000000000, 0.000000000000000000, 1.000000000000000000 ) ) ;
#19808 = DIRECTION ( 'NONE',  ( -1.000000000000000000, 0.000000000000000000, 0.000000000000000000 ) ) ;
#19809 = LINE ( 'NONE', #13065, #11057 ) ;
#19810 = CARTESIAN_POINT ( 'NONE',  ( 0.000000000000000000, 30.61448696004464409, -9.314139153633924195 ) ) ;
#19811 = CARTESIAN_POINT ( 'NONE',  ( 10.00000000000000000, -70.37753541435900217, -60.02863908169706519 ) ) ;
#19812 = DIRECTION ( 'NONE',  ( -1.000000000000000000, 0.000000000000000000, 0.000000000000000000 ) ) ;
#19813 = DIRECTION ( 'NONE',  ( 1.000000000000000000, 0.000000000000000000, 0.000000000000000000 ) ) ;
#19814 = CARTESIAN_POINT ( 'NONE',  ( 10.00000000000000000, -66.01871308925419157, -64.79170103523090063 ) ) ;
#19815 = ORIENTED_EDGE ( 'NONE', *, *, #13496, .F. ) ;
#19816 = ORIENTED_EDGE ( 'NONE', *, *, #10099, .T. ) ;
#19817 = DIRECTION ( 'NONE',  ( -1.000000000000000000, 0.000000000000000000, 0.000000000000000000 ) ) ;
#19818 = EDGE_CURVE ( 'NONE', #971, #1435, #8663, .T. ) ;
#19819 = CIRCLE ( 'NONE', #18774, 44.99999999999998579 ) ;
#19820 = LINE ( 'NONE', #13180, #4936 ) ;
#19821 = ORIENTED_EDGE ( 'NONE', *, *, #3334, .F. ) ;
#19822 = ORIENTED_EDGE ( 'NONE', *, *, #6494, .T. ) ;
#19823 = ORIENTED_EDGE ( 'NONE', *, *, #2884, .F. ) ;
#19824 = ORIENTED_EDGE ( 'NONE', *, *, #4594, .T. ) ;
#19825 = DIRECTION ( 'NONE',  ( 1.000000000000000000, 0.000000000000000000, 0.000000000000000000 ) ) ;
#19826 = DIRECTION ( 'NONE',  ( 0.000000000000000000, 0.000000000000000000, -1.000000000000000000 ) ) ;
#19827 = EDGE_CURVE ( 'NONE', #12369, #9115, #3729, .T. ) ;
#19828 = ORIENTED_EDGE ( 'NONE', *, *, #14309, .F. ) ;
#19829 = CYLINDRICAL_SURFACE ( 'NONE', #2254, 44.99999999999999289 ) ;
#19830 = FACE_OUTER_BOUND ( 'NONE', #12647, .T. ) ;
#19831 = CARTESIAN_POINT ( 'NONE',  ( 5.000000000000000000, -23.37352460145298139, 21.85585385440871775 ) ) ;
#19832 = CARTESIAN_POINT ( 'NONE',  ( 10.00000000000000000, 75.45728100697654384, -39.26051685138985903 ) ) ;
#19833 = CYLINDRICAL_SURFACE ( 'NONE', #21644, 92.50100000000000477 ) ;
#19834 = CYLINDRICAL_SURFACE ( 'NONE', #16617, 92.50100000000000477 ) ;
#19835 = UNCERTAINTY_MEASURE_WITH_UNIT (LENGTH_MEASURE( 1.000000000000000082E-05 ), #9316, 'distance_accuracy_value', 'NONE');
#19836 = ORIENTED_EDGE ( 'NONE', *, *, #2283, .T. ) ;
#19837 = CARTESIAN_POINT ( 'NONE',  ( 7.999999999999986677, 113.8250000000000171, 0.000000000000000000 ) ) ;
#19838 = CIRCLE ( 'NONE', #21607, 45.00000000000000000 ) ;
#19839 = CARTESIAN_POINT ( 'NONE',  ( 0.000000000000000000, -21.31452625070873452, -82.34610137166143318 ) ) ;
#19840 = ORIENTED_EDGE ( 'NONE', *, *, #9839, .F. ) ;
#19841 = DIRECTION ( 'NONE',  ( -1.000000000000000000, -0.000000000000000000, -0.000000000000000000 ) ) ;
#19842 = EDGE_LOOP ( 'NONE', ( #18040, #9847, #15726, #4143 ) ) ;
#19843 = AXIS2_PLACEMENT_3D ( 'NONE', #18241, #18683, #20219 ) ;
#19844 = DIRECTION ( 'NONE',  ( 0.000000000000000000, -0.6427876096865300370, -0.7660444431189857850 ) ) ;
#19845 = EDGE_CURVE ( 'NONE', #7162, #15664, #5138, .T. ) ;
#19846 = EDGE_CURVE ( 'NONE', #14785, #17245, #16068, .T. ) ;
#19847 = EDGE_CURVE ( 'NONE', #10308, #13383, #15504, .T. ) ;
#19848 = CARTESIAN_POINT ( 'NONE',  ( -10.00000000000000000, 0.000000000000000000, 0.000000000000000000 ) ) ;
#19849 = VERTEX_POINT ( 'NONE', #7114 ) ;
#19850 = CIRCLE ( 'NONE', #15253, 27.49900000000000233 ) ;
#19851 = CARTESIAN_POINT ( 'NONE',  ( 10.00000000000000000, -84.19736439813830486, 38.30455363800902546 ) ) ;
#19852 = EDGE_CURVE ( 'NONE', #19022, #13874, #8320, .T. ) ;
#19853 = VERTEX_POINT ( 'NONE', #13741 ) ;
#19854 = ORIENTED_EDGE ( 'NONE', *, *, #20647, .T. ) ;
#19855 = DIRECTION ( 'NONE',  ( 0.000000000000000000, 0.000000000000000000, 1.000000000000000000 ) ) ;
#19856 = ORIENTED_EDGE ( 'NONE', *, *, #15551, .T. ) ;
#19857 = CARTESIAN_POINT ( 'NONE',  ( -10.00000000000000000, 0.000000000000000000, 0.000000000000000000 ) ) ;
#19858 = TOROIDAL_SURFACE ( 'NONE', #1862, 101.1000000000000369, 1.100000000000002087 ) ;
#19859 = CARTESIAN_POINT ( 'NONE',  ( 10.00000000000000000, -92.49798535263880694, 0.7467976319017460840 ) ) ;
#19860 = LINE ( 'NONE', #11905, #17013 ) ;
#19861 = FILL_AREA_STYLE ('',( #4844 ) ) ;
#19862 = ADVANCED_FACE ( 'NONE', ( #20485 ), #5128, .F. ) ;
#19863 = CIRCLE ( 'NONE', #5041, 88.00000000000000000 ) ;
#19864 = DIRECTION ( 'NONE',  ( 1.000000000000000000, 0.000000000000000000, 0.000000000000000000 ) ) ;
#19865 = DIRECTION ( 'NONE',  ( -1.000000000000000000, 0.000000000000000000, -0.000000000000000000 ) ) ;
#19866 = CIRCLE ( 'NONE', #5066, 44.99999999999998579 ) ;
#19867 = DIRECTION ( 'NONE',  ( 1.000000000000000000, 0.000000000000000000, 0.000000000000000000 ) ) ;
#19868 = ADVANCED_FACE ( 'NONE', ( #18822 ), #18610, .F. ) ;
#19869 = CARTESIAN_POINT ( 'NONE',  ( 0.000000000000000000, -65.64563793391792501, -54.09103124042881916 ) ) ;
#19870 = AXIS2_PLACEMENT_3D ( 'NONE', #2876, #202, #8294 ) ;
#19871 = FACE_OUTER_BOUND ( 'NONE', #3791, .T. ) ;
#19872 = CARTESIAN_POINT ( 'NONE',  ( 10.00000000000000000, 41.21966518005955038, 82.80926399530301296 ) ) ;
#19873 = ORIENTED_EDGE ( 'NONE', *, *, #2990, .F. ) ;
#19874 = CIRCLE ( 'NONE', #8238, 44.99999999999999289 ) ;
#19875 = ORIENTED_EDGE ( 'NONE', *, *, #6387, .T. ) ;
#19876 = ORIENTED_EDGE ( 'NONE', *, *, #3958, .T. ) ;
#19877 = AXIS2_PLACEMENT_3D ( 'NONE', #11437, #17671, #8138 ) ;
#19878 = ADVANCED_FACE ( 'NONE', ( #14268 ), #21238, .F. ) ;
#19879 = EDGE_LOOP ( 'NONE', ( #13163, #11890, #4938, #4228 ) ) ;
#19880 = AXIS2_PLACEMENT_3D ( 'NONE', #4561, #5895, #4233 ) ;
#19881 = ORIENTED_EDGE ( 'NONE', *, *, #19846, .F. ) ;
#19882 = DIRECTION ( 'NONE',  ( 0.000000000000000000, 0.000000000000000000, -1.000000000000000000 ) ) ;
#19883 = CIRCLE ( 'NONE', #17777, 92.50100000000000477 ) ;
#19884 = ORIENTED_EDGE ( 'NONE', *, *, #16216, .T. ) ;
#19885 = DIRECTION ( 'NONE',  ( 0.000000000000000000, 0.000000000000000000, 1.000000000000000000 ) ) ;
#19886 = LINE ( 'NONE', #4753, #16321 ) ;
#19887 = ADVANCED_FACE ( 'NONE', ( #2792 ), #7769, .F. ) ;
#19888 = CIRCLE ( 'NONE', #10009, 44.99999999999999289 ) ;
#19889 = CARTESIAN_POINT ( 'NONE',  ( 0.000000000000000000, -46.89573839703219704, -79.73220629831536144 ) ) ;
#19890 = DIRECTION ( 'NONE',  ( -1.000000000000000000, -0.000000000000000000, 0.000000000000000000 ) ) ;
#19891 = DIRECTION ( 'NONE',  ( -1.000000000000000000, -0.000000000000000000, -0.000000000000000000 ) ) ;
#19892 = EDGE_CURVE ( 'NONE', #12050, #6056, #10425, .T. ) ;
#19893 = LINE ( 'NONE', #8297, #10470 ) ;
#19894 = DIRECTION ( 'NONE',  ( -1.000000000000000000, 0.000000000000000000, 0.000000000000000000 ) ) ;
#19895 = VECTOR ( 'NONE', #1038, 1000.000000000000000 ) ;
#19896 = EDGE_CURVE ( 'NONE', #8175, #3440, #14500, .T. ) ;
#19897 = VERTEX_POINT ( 'NONE', #19578 ) ;
#19898 = AXIS2_PLACEMENT_3D ( 'NONE', #7684, #4591, #6260 ) ;
#19899 = ADVANCED_FACE ( 'NONE', ( #14386 ), #10959, .F. ) ;
#19900 = DIRECTION ( 'NONE',  ( 1.000000000000000000, -0.000000000000000000, 0.000000000000000000 ) ) ;
#19901 = ORIENTED_EDGE ( 'NONE', *, *, #16228, .F. ) ;
#19902 = ORIENTED_EDGE ( 'NONE', *, *, #21203, .T. ) ;
#19903 = CARTESIAN_POINT ( 'NONE',  ( 0.000000000000000000, -57.47876254627099257, -62.70072803846446163 ) ) ;
#19904 = CIRCLE ( 'NONE', #17453, 44.99999999999999289 ) ;
#19905 = EDGE_CURVE ( 'NONE', #1976, #18330, #17491, .T. ) ;
#19906 = ORIENTED_EDGE ( 'NONE', *, *, #19018, .T. ) ;
#19907 = DIRECTION ( 'NONE',  ( 0.000000000000000000, 0.000000000000000000, 1.000000000000000000 ) ) ;
#19908 = ORIENTED_EDGE ( 'NONE', *, *, #1411, .F. ) ;
#19909 = ORIENTED_EDGE ( 'NONE', *, *, #8354, .F. ) ;
#19910 = APPLICATION_PROTOCOL_DEFINITION ( 'draft international standard', 'automotive_design', 1998, #18859 ) ;
#19911 = CIRCLE ( 'NONE', #18861, 32.00000000000000000 ) ;
#19912 = LINE ( 'NONE', #4890, #290 ) ;
#19913 = ORIENTED_EDGE ( 'NONE', *, *, #16209, .F. ) ;
#19914 = CARTESIAN_POINT ( 'NONE',  ( -90.00000000000000000, 0.000000000000000000, -113.8250000000000171 ) ) ;
#19915 = AXIS2_PLACEMENT_3D ( 'NONE', #2468, #3797, #9193 ) ;
#19916 = CARTESIAN_POINT ( 'NONE',  ( -1.500000000000001332, 0.000000000000000000, 0.000000000000000000 ) ) ;
#19917 = DIRECTION ( 'NONE',  ( 0.000000000000000000, 0.000000000000000000, -1.000000000000000000 ) ) ;
#19918 = DIRECTION ( 'NONE',  ( 0.000000000000000000, -0.9848077530122062440, -0.1736481776669404897 ) ) ;
#19919 = DIRECTION ( 'NONE',  ( -1.000000000000000000, -0.000000000000000000, -0.000000000000000000 ) ) ;
#19920 = CARTESIAN_POINT ( 'NONE',  ( 0.000000000000000000, 0.000000000000000000, 3.000000000000000000 ) ) ;
#19921 = CYLINDRICAL_SURFACE ( 'NONE', #19971, 44.99999999999999289 ) ;
#19922 = DIRECTION ( 'NONE',  ( 0.000000000000000000, 0.000000000000000000, 1.000000000000000000 ) ) ;
#19923 = AXIS2_PLACEMENT_3D ( 'NONE', #20453, #13910, #17349 ) ;
#19924 = AXIS2_PLACEMENT_3D ( 'NONE', #18110, #21636, #6308 ) ;
#19925 = ORIENTED_EDGE ( 'NONE', *, *, #12322, .T. ) ;
#19926 = VECTOR ( 'NONE', #2142, 1000.000000000000000 ) ;
#19927 = CIRCLE ( 'NONE', #4410, 44.99999999999999289 ) ;
#19928 = CYLINDRICAL_SURFACE ( 'NONE', #20407, 32.00000000000000000 ) ;
#19929 = FACE_OUTER_BOUND ( 'NONE', #1027, .T. ) ;
#19930 = ORIENTED_EDGE ( 'NONE', *, *, #18953, .F. ) ;
#19931 = FACE_OUTER_BOUND ( 'NONE', #10328, .T. ) ;
#19932 = ORIENTED_EDGE ( 'NONE', *, *, #12846, .F. ) ;
#19933 =( NAMED_UNIT ( * ) PLANE_ANGLE_UNIT ( ) SI_UNIT ( $, .RADIAN. ) );
#19934 = AXIS2_PLACEMENT_3D ( 'NONE', #9686, #9249, #14461 ) ;
#19935 = ORIENTED_EDGE ( 'NONE', *, *, #939, .T. ) ;
#19936 = CARTESIAN_POINT ( 'NONE',  ( -10.00000000000000000, 0.000000000000000000, 0.000000000000000000 ) ) ;
#19937 = ORIENTED_EDGE ( 'NONE', *, *, #2575, .F. ) ;
#19938 = VECTOR ( 'NONE', #12765, 1000.000000000000000 ) ;
#19939 = ORIENTED_EDGE ( 'NONE', *, *, #20276, .F. ) ;
#19940 = DIRECTION ( 'NONE',  ( 0.000000000000000000, 0.9945218953682736229, -0.1045284632676503761 ) ) ;
#19941 = CARTESIAN_POINT ( 'NONE',  ( 0.000000000000000000, 5.000000000000000000, 0.000000000000000000 ) ) ;
#19942 = ORIENTED_EDGE ( 'NONE', *, *, #4096, .F. ) ;
#19943 = CIRCLE ( 'NONE', #4419, 88.00000000000000000 ) ;
#19944 = DIRECTION ( 'NONE',  ( -0.000000000000000000, -1.000000000000000000, -0.000000000000000000 ) ) ;
#19945 = DIRECTION ( 'NONE',  ( 0.000000000000000000, 0.000000000000000000, 1.000000000000000000 ) ) ;
#19946 = CARTESIAN_POINT ( 'NONE',  ( 10.00000000000000000, 0.000000000000000000, 0.000000000000000000 ) ) ;
#19947 = CARTESIAN_POINT ( 'NONE',  ( -90.00000000000000000, 8.239576745513313235E-16, 6.728125000000022560 ) ) ;
#19948 = CIRCLE ( 'NONE', #3717, 88.00000000000000000 ) ;
#19949 = CARTESIAN_POINT ( 'NONE',  ( 10.00000000000000000, 48.19312842678564834, -70.09002648625148879 ) ) ;
#19950 = DIRECTION ( 'NONE',  ( 0.000000000000000000, 0.000000000000000000, 1.000000000000000000 ) ) ;
#19951 = ADVANCED_FACE ( 'NONE', ( #587 ), #16154, .T. ) ;
#19952 = AXIS2_PLACEMENT_3D ( 'NONE', #4592, #13420, #6590 ) ;
#19953 = VERTEX_POINT ( 'NONE', #6009 ) ;
#19954 = DIRECTION ( 'NONE',  ( 0.000000000000000000, 0.000000000000000000, 1.000000000000000000 ) ) ;
#19955 = DIRECTION ( 'NONE',  ( 0.000000000000000000, -0.8290375725550469532, 0.5591929034707392443 ) ) ;
#19956 = ORIENTED_EDGE ( 'NONE', *, *, #5692, .F. ) ;
#19957 = AXIS2_PLACEMENT_3D ( 'NONE', #16741, #16305, #21828 ) ;
#19958 = AXIS2_PLACEMENT_3D ( 'NONE', #15172, #14951, #13412 ) ;
#19959 = EDGE_CURVE ( 'NONE', #6202, #589, #12829, .T. ) ;
#19960 = CIRCLE ( 'NONE', #8321, 44.99999999999999289 ) ;
#19961 = CYLINDRICAL_SURFACE ( 'NONE', #18969, 11.99999999999999645 ) ;
#19962 = AXIS2_PLACEMENT_3D ( 'NONE', #1006, #4542, #14812 ) ;
#19963 = ORIENTED_EDGE ( 'NONE', *, *, #15816, .F. ) ;
#19964 = DIRECTION ( 'NONE',  ( -1.000000000000000000, 0.000000000000000000, 0.000000000000000000 ) ) ;
#19965 = DIRECTION ( 'NONE',  ( -1.000000000000000000, -0.000000000000000000, -0.000000000000000000 ) ) ;
#19966 = VERTEX_POINT ( 'NONE', #10739 ) ;
#19967 = DIRECTION ( 'NONE',  ( 0.000000000000000000, -0.7431448254773999063, 0.6691306063588519093 ) ) ;
#19968 = ORIENTED_EDGE ( 'NONE', *, *, #3044, .T. ) ;
#19969 = EDGE_LOOP ( 'NONE', ( #2201, #5598 ) ) ;
#19970 = DIRECTION ( 'NONE',  ( -1.000000000000000000, 0.000000000000000000, 0.000000000000000000 ) ) ;
#19971 = AXIS2_PLACEMENT_3D ( 'NONE', #9746, #4793, #13070 ) ;
#19972 = ORIENTED_EDGE ( 'NONE', *, *, #20181, .F. ) ;
#19973 = DIRECTION ( 'NONE',  ( 0.000000000000000000, 0.000000000000000000, 1.000000000000000000 ) ) ;
#19974 = CARTESIAN_POINT ( 'NONE',  ( 0.000000000000000000, -31.15801000616779248, -79.14775961996421927 ) ) ;
#19975 = DIRECTION ( 'NONE',  ( 0.000000000000000000, 0.000000000000000000, -1.000000000000000000 ) ) ;
#19976 = VECTOR ( 'NONE', #16360, 1000.000000000000000 ) ;
#19977 = CARTESIAN_POINT ( 'NONE',  ( 10.00000000000000000, 0.000000000000000000, 0.000000000000000000 ) ) ;
#19978 = AXIS2_PLACEMENT_3D ( 'NONE', #8852, #12379, #19025 ) ;
#19979 = FACE_OUTER_BOUND ( 'NONE', #9530, .T. ) ;
#19980 = AXIS2_PLACEMENT_3D ( 'NONE', #7780, #2247, #11193 ) ;
#19981 = AXIS2_PLACEMENT_3D ( 'NONE', #20686, #7427, #17270 ) ;
#19982 = EDGE_CURVE ( 'NONE', #6262, #17309, #18202, .T. ) ;
#19983 = CARTESIAN_POINT ( 'NONE',  ( 10.00000000000000000, -48.19312842678424857, -70.09002648625245513 ) ) ;
#19984 = EDGE_CURVE ( 'NONE', #13200, #15636, #8118, .T. ) ;
#19985 = DIRECTION ( 'NONE',  ( -1.000000000000000000, 0.000000000000000000, 0.000000000000000000 ) ) ;
#19986 = CARTESIAN_POINT ( 'NONE',  ( 0.000000000000000000, -69.25892805976543798, 49.38005998797819274 ) ) ;
#19987 = DIRECTION ( 'NONE',  ( 0.000000000000000000, 0.000000000000000000, 1.000000000000000000 ) ) ;
#19988 = DIRECTION ( 'NONE',  ( 0.000000000000000000, -0.7431448254774000173, 0.6691306063588519093 ) ) ;
#19989 = EDGE_LOOP ( 'NONE', ( #15772, #2114, #8890, #21672 ) ) ;
#19990 = AXIS2_PLACEMENT_3D ( 'NONE', #21559, #4983, #16806 ) ;
#19991 = ORIENTED_EDGE ( 'NONE', *, *, #8257, .T. ) ;
#19992 = AXIS2_PLACEMENT_3D ( 'NONE', #19030, #17800, #11049 ) ;
#19993 = ORIENTED_EDGE ( 'NONE', *, *, #9480, .T. ) ;
#19994 = AXIS2_PLACEMENT_3D ( 'NONE', #6325, #8077, #14813 ) ;
#19995 = EDGE_CURVE ( 'NONE', #11594, #1127, #12997, .T. ) ;
#19996 = ORIENTED_EDGE ( 'NONE', *, *, #3650, .F. ) ;
#19997 = ORIENTED_EDGE ( 'NONE', *, *, #2455, .F. ) ;
#19998 = EDGE_CURVE ( 'NONE', #15560, #6332, #4327, .T. ) ;
#19999 = DIRECTION ( 'NONE',  ( 0.000000000000000000, -0.1391731009600519209, -0.9902680687415721383 ) ) ;
#20000 = ORIENTED_EDGE ( 'NONE', *, *, #11246, .F. ) ;
#20001 = DIRECTION ( 'NONE',  ( 0.000000000000000000, 0.000000000000000000, 1.000000000000000000 ) ) ;
#20002 = CARTESIAN_POINT ( 'NONE',  ( 5.000000000000002665, 11.59241532900628258, 87.23311244498744088 ) ) ;
#20003 = AXIS2_PLACEMENT_3D ( 'NONE', #14918, #4980, #2988 ) ;
#20004 = ADVANCED_FACE ( 'NONE', ( #11067 ), #17816, .F. ) ;
#20005 = CARTESIAN_POINT ( 'NONE',  ( 0.000000000000000000, 0.000000000000000000, 0.000000000000000000 ) ) ;
#20006 = CIRCLE ( 'NONE', #1303, 44.99999999999999289 ) ;
#20007 = CARTESIAN_POINT ( 'NONE',  ( 10.00000000000000000, 0.000000000000000000, 0.000000000000000000 ) ) ;
#20008 = EDGE_CURVE ( 'NONE', #20663, #16623, #17499, .T. ) ;
#20009 = AXIS2_PLACEMENT_3D ( 'NONE', #1527, #9809, #5070 ) ;
#20010 = CARTESIAN_POINT ( 'NONE',  ( -9.999999999999998224, 0.000000000000000000, 3.000000000000000000 ) ) ;
#20011 = EDGE_CURVE ( 'NONE', #4316, #14805, #15110, .T. ) ;
#20012 = AXIS2_PLACEMENT_3D ( 'NONE', #1989, #13368, #4979 ) ;
#20013 = DIRECTION ( 'NONE',  ( -1.000000000000000000, -0.000000000000000000, 0.000000000000000000 ) ) ;
#20014 = DIRECTION ( 'NONE',  ( 0.000000000000000000, 0.000000000000000000, 1.000000000000000000 ) ) ;
#20015 = EDGE_CURVE ( 'NONE', #11182, #6332, #14773, .T. ) ;
#20016 = ORIENTED_EDGE ( 'NONE', *, *, #20082, .F. ) ;
#20017 = CARTESIAN_POINT ( 'NONE',  ( 0.000000000000000000, 68.36541360927260769, -50.60987712331631627 ) ) ;
#20018 = EDGE_LOOP ( 'NONE', ( #9560, #9730, #9191, #3249 ) ) ;
#20019 = ORIENTED_EDGE ( 'NONE', *, *, #9707, .T. ) ;
#20020 = EDGE_CURVE ( 'NONE', #9215, #18973, #4185, .T. ) ;
#20021 = CIRCLE ( 'NONE', #8728, 92.50100000000000477 ) ;
#20022 = DIRECTION ( 'NONE',  ( 0.000000000000000000, 1.000000000000000000, -1.224646799147353207E-16 ) ) ;
#20023 = ORIENTED_EDGE ( 'NONE', *, *, #20276, .T. ) ;
#20024 = DIRECTION ( 'NONE',  ( 0.000000000000000000, 0.000000000000000000, -1.000000000000000000 ) ) ;
#20025 = EDGE_LOOP ( 'NONE', ( #11290, #13631, #12499, #2090 ) ) ;
#20026 = ADVANCED_FACE ( 'NONE', ( #7982 ), #6444, .F. ) ;
#20027 = EDGE_LOOP ( 'NONE', ( #1671, #14421, #21145, #6141 ) ) ;
#20028 = CYLINDRICAL_SURFACE ( 'NONE', #16861, 11.99999999999999822 ) ;
#20029 = ORIENTED_EDGE ( 'NONE', *, *, #6143, .T. ) ;
#20030 = DIRECTION ( 'NONE',  ( -1.000000000000000000, 0.000000000000000000, 0.000000000000000000 ) ) ;
#20031 = DIRECTION ( 'NONE',  ( 0.000000000000000000, 0.9945218953682736229, -0.1045284632676503622 ) ) ;
#20032 = EDGE_CURVE ( 'NONE', #1246, #4660, #1014, .T. ) ;
#20033 = CARTESIAN_POINT ( 'NONE',  ( 10.00000000000000000, -92.49798535263882115, -0.7467976319030308341 ) ) ;
#20034 = DIRECTION ( 'NONE',  ( 1.000000000000000000, 0.000000000000000000, 0.000000000000000000 ) ) ;
#20035 = CARTESIAN_POINT ( 'NONE',  ( 0.000000000000000000, -31.75612719289738095, -3.943144139962873940 ) ) ;
#20036 = CARTESIAN_POINT ( 'NONE',  ( 5.000000000000000888, 6.063030049135073263, 31.42037024962127134 ) ) ;
#20037 = DIRECTION ( 'NONE',  ( 0.000000000000000000, 0.000000000000000000, 1.000000000000000000 ) ) ;
#20038 = AXIS2_PLACEMENT_3D ( 'NONE', #14143, #7197, #15481 ) ;
#20039 = EDGE_CURVE ( 'NONE', #10149, #5754, #14714, .T. ) ;
#20040 = AXIS2_PLACEMENT_3D ( 'NONE', #17520, #17733, #11205 ) ;
#20041 = AXIS2_PLACEMENT_3D ( 'NONE', #19181, #7579, #14315 ) ;
#20042 = ORIENTED_EDGE ( 'NONE', *, *, #9072, .T. ) ;
#20043 = VECTOR ( 'NONE', #16607, 1000.000000000000000 ) ;
#20044 = DIRECTION ( 'NONE',  ( 0.000000000000000000, 0.000000000000000000, 1.000000000000000000 ) ) ;
#20045 = LINE ( 'NONE', #13296, #21526 ) ;
#20046 = ORIENTED_EDGE ( 'NONE', *, *, #13110, .T. ) ;
#20047 = DIRECTION ( 'NONE',  ( -1.000000000000000000, -0.000000000000000000, -0.000000000000000000 ) ) ;
#20048 = EDGE_CURVE ( 'NONE', #3139, #13772, #6662, .T. ) ;
#20049 = VERTEX_POINT ( 'NONE', #15042 ) ;
#20050 = VECTOR ( 'NONE', #5758, 1000.000000000000000 ) ;
#20051 = VECTOR ( 'NONE', #20597, 1000.000000000000000 ) ;
#20052 = EDGE_LOOP ( 'NONE', ( #10445, #1918, #10551, #5981 ) ) ;
#20053 = DIRECTION ( 'NONE',  ( 0.000000000000000000, 0.000000000000000000, 1.000000000000000000 ) ) ;
#20054 = ORIENTED_EDGE ( 'NONE', *, *, #1249, .F. ) ;
#20055 = ORIENTED_EDGE ( 'NONE', *, *, #9365, .T. ) ;
#20056 = DIRECTION ( 'NONE',  ( 0.000000000000000000, 0.000000000000000000, -1.000000000000000000 ) ) ;
#20057 = CARTESIAN_POINT ( 'NONE',  ( 10.00000000000000000, -71.33759994382000968, 58.88447872958963814 ) ) ;
#20058 = AXIS2_PLACEMENT_3D ( 'NONE', #7853, #4651, #16683 ) ;
#20059 = ORIENTED_EDGE ( 'NONE', *, *, #20748, .F. ) ;
#20060 = EDGE_CURVE ( 'NONE', #3222, #9874, #19799, .T. ) ;
#20061 = CARTESIAN_POINT ( 'NONE',  ( 0.000000000000000000, -3.786343810537388332, -27.23708136986056161 ) ) ;
#20062 = CARTESIAN_POINT ( 'NONE',  ( -10.00000000000000000, 0.000000000000000000, 0.000000000000000000 ) ) ;
#20063 = DIRECTION ( 'NONE',  ( -1.000000000000000000, -0.000000000000000000, -0.000000000000000000 ) ) ;
#20064 = DIRECTION ( 'NONE',  ( -1.000000000000000000, 0.000000000000000000, 0.000000000000000000 ) ) ;
#20065 = DIRECTION ( 'NONE',  ( 0.000000000000000000, 0.000000000000000000, 1.000000000000000000 ) ) ;
#20066 = CYLINDRICAL_SURFACE ( 'NONE', #14849, 32.00000000000000000 ) ;
#20067 = UNCERTAINTY_MEASURE_WITH_UNIT (LENGTH_MEASURE( 1.000000000000000082E-05 ), #9761, 'distance_accuracy_value', 'NONE');
#20068 = ORIENTED_EDGE ( 'NONE', *, *, #7761, .T. ) ;
#20069 = CARTESIAN_POINT ( 'NONE',  ( 0.000000000000000000, 48.19312842678472464, 70.09002648625214249 ) ) ;
#20070 = CIRCLE ( 'NONE', #2091, 88.00000000000000000 ) ;
#20071 = CARTESIAN_POINT ( 'NONE',  ( 10.00000000000000000, -25.48117629651196125, 10.33947075754252332 ) ) ;
#20072 = VECTOR ( 'NONE', #12719, 1000.000000000000000 ) ;
#20073 = ORIENTED_EDGE ( 'NONE', *, *, #20416, .F. ) ;
#20074 = AXIS2_PLACEMENT_3D ( 'NONE', #14916, #9938, #18360 ) ;
#20075 = CIRCLE ( 'NONE', #6317, 88.00000000000000000 ) ;
#20076 = AXIS2_PLACEMENT_3D ( 'NONE', #603, #14079, #2250 ) ;
#20077 = CIRCLE ( 'NONE', #10535, 27.49900000000000233 ) ;
#20078 = DIRECTION ( 'NONE',  ( 1.000000000000000000, 0.000000000000000000, 0.000000000000000000 ) ) ;
#20079 = EDGE_LOOP ( 'NONE', ( #10608, #2834, #19884, #3393 ) ) ;
#20080 = FILL_AREA_STYLE ('',( #21724 ) ) ;
#20081 = DIRECTION ( 'NONE',  ( 0.000000000000000000, 0.000000000000000000, 1.000000000000000000 ) ) ;
#20082 = EDGE_CURVE ( 'NONE', #19773, #1794, #19355, .T. ) ;
#20083 = ORIENTED_EDGE ( 'NONE', *, *, #12217, .F. ) ;
#20084 = CARTESIAN_POINT ( 'NONE',  ( 0.000000000000000000, 24.17932380791719282, 20.96092317127012805 ) ) ;
#20085 = VERTEX_POINT ( 'NONE', #7867 ) ;
#20086 = VERTEX_POINT ( 'NONE', #9612 ) ;
#20087 = CARTESIAN_POINT ( 'NONE',  ( 0.000000000000000000, 0.000000000000000000, 0.000000000000000000 ) ) ;
#20088 = ORIENTED_EDGE ( 'NONE', *, *, #13126, .T. ) ;
#20089 = CARTESIAN_POINT ( 'NONE',  ( 10.00000000000000000, -13.56333590713994575, -28.98337314858448366 ) ) ;
#20090 = AXIS2_PLACEMENT_3D ( 'NONE', #9911, #14889, #19760 ) ;
#20091 = DIRECTION ( 'NONE',  ( 1.000000000000000000, 0.000000000000000000, 0.000000000000000000 ) ) ;
#20092 = DIRECTION ( 'NONE',  ( -1.000000000000000000, -0.000000000000000000, 0.000000000000000000 ) ) ;
#20093 = VECTOR ( 'NONE', #8359, 1000.000000000000000 ) ;
#20094 = DIRECTION ( 'NONE',  ( 1.000000000000000000, -0.000000000000000000, -0.000000000000000000 ) ) ;
#20095 = AXIS2_PLACEMENT_3D ( 'NONE', #17656, #5618, #636 ) ;
#20096 = CIRCLE ( 'NONE', #15491, 92.50100000000000477 ) ;
#20097 = DIRECTION ( 'NONE',  ( 1.000000000000000000, 0.000000000000000000, 0.000000000000000000 ) ) ;
#20098 = DIRECTION ( 'NONE',  ( 0.000000000000000000, 0.000000000000000000, -1.000000000000000000 ) ) ;
#20099 = CARTESIAN_POINT ( 'NONE',  ( 0.000000000000000000, 0.000000000000000000, 0.000000000000000000 ) ) ;
#20100 = CARTESIAN_POINT ( 'NONE',  ( -10.00000000000000000, 0.000000000000000000, 0.000000000000000000 ) ) ;
#20101 = DIRECTION ( 'NONE',  ( 0.000000000000000000, 0.000000000000000000, 1.000000000000000000 ) ) ;
#20102 = VECTOR ( 'NONE', #7211, 1000.000000000000000 ) ;
#20103 = DIRECTION ( 'NONE',  ( 0.000000000000000000, -0.2079116908177469081, -0.9781476007338082423 ) ) ;
#20104 = AXIS2_PLACEMENT_3D ( 'NONE', #5279, #17092, #80 ) ;
#20105 = ORIENTED_EDGE ( 'NONE', *, *, #11797, .F. ) ;
#20106 = CARTESIAN_POINT ( 'NONE',  ( 123.0000000000000000, 0.000000000000000000, -3.000000000000000000 ) ) ;
#20107 = AXIS2_PLACEMENT_3D ( 'NONE', #15630, #3926, #10233 ) ;
#20108 = ORIENTED_EDGE ( 'NONE', *, *, #4363, .F. ) ;
#20109 = PRESENTATION_LAYER_ASSIGNMENT (  '', '', ( #17280 ) ) ;
#20110 = AXIS2_PLACEMENT_3D ( 'NONE', #9338, #5934, #19187 ) ;
#20111 = ORIENTED_EDGE ( 'NONE', *, *, #20414, .F. ) ;
#20112 = VERTEX_POINT ( 'NONE', #4556 ) ;
#20113 = EDGE_CURVE ( 'NONE', #10715, #19331, #9819, .T. ) ;
#20114 = ORIENTED_EDGE ( 'NONE', *, *, #16743, .T. ) ;
#20115 = CARTESIAN_POINT ( 'NONE',  ( 10.00000000000000000, 0.000000000000000000, 0.000000000000000000 ) ) ;
#20116 = VERTEX_POINT ( 'NONE', #16594 ) ;
#20117 = CYLINDRICAL_SURFACE ( 'NONE', #1854, 44.99999999999999289 ) ;
#20118 = CARTESIAN_POINT ( 'NONE',  ( 10.00000000000000000, 0.000000000000000000, 0.000000000000000000 ) ) ;
#20119 = EDGE_CURVE ( 'NONE', #10039, #12967, #11397, .T. ) ;
#20120 = DIRECTION ( 'NONE',  ( 0.000000000000000000, 0.000000000000000000, 1.000000000000000000 ) ) ;
#20121 = DIRECTION ( 'NONE',  ( -1.000000000000000000, -0.000000000000000000, 0.000000000000000000 ) ) ;
#20122 = CIRCLE ( 'NONE', #9501, 45.00000000000000000 ) ;
#20123 = CARTESIAN_POINT ( 'NONE',  ( 0.000000000000000000, -7.619321854369379032, -26.42235673590698397 ) ) ;
#20124 = EDGE_CURVE ( 'NONE', #5926, #10821, #16170, .T. ) ;
#20125 = CARTESIAN_POINT ( 'NONE',  ( 10.00000000000000000, -68.93609746931198856, 54.69748134696436637 ) ) ;
#20126 = ORIENTED_EDGE ( 'NONE', *, *, #11338, .T. ) ;
#20127 = FACE_OUTER_BOUND ( 'NONE', #16574, .T. ) ;
#20128 = ORIENTED_EDGE ( 'NONE', *, *, #21621, .F. ) ;
#20129 = ORIENTED_EDGE ( 'NONE', *, *, #3615, .F. ) ;
#20130 = CARTESIAN_POINT ( 'NONE',  ( 0.000000000000000000, 52.25832601289098278, 70.80301803122803506 ) ) ;
#20131 = EDGE_CURVE ( 'NONE', #21840, #14663, #2078, .T. ) ;
#20132 = ORIENTED_EDGE ( 'NONE', *, *, #8798, .F. ) ;
#20133 = EDGE_CURVE ( 'NONE', #16928, #3486, #15826, .T. ) ;
#20134 = ADVANCED_FACE ( 'NONE', ( #21565 ), #11514, .F. ) ;
#20135 = CIRCLE ( 'NONE', #15538, 44.99999999999998579 ) ;
#20136 = CARTESIAN_POINT ( 'NONE',  ( 10.00000000000000000, 9.646732466565339337, 84.51112348751853176 ) ) ;
#20137 = EDGE_LOOP ( 'NONE', ( #19048, #7834, #10063, #11629 ) ) ;
#20138 = ORIENTED_EDGE ( 'NONE', *, *, #6219, .T. ) ;
#20139 = DIRECTION ( 'NONE',  ( -1.000000000000000000, -0.000000000000000000, -0.000000000000000000 ) ) ;
#20140 = EDGE_CURVE ( 'NONE', #1976, #6010, #9451, .T. ) ;
#20141 = ORIENTED_EDGE ( 'NONE', *, *, #15816, .T. ) ;
#20142 = CARTESIAN_POINT ( 'NONE',  ( 0.000000000000000000, -89.12061559554348378, 24.77803214283513356 ) ) ;
#20143 = DIRECTION ( 'NONE',  ( 0.000000000000000000, -1.850371707708594444E-14, -1.000000000000000000 ) ) ;
#20144 = DIRECTION ( 'NONE',  ( 1.000000000000000000, 0.000000000000000000, 0.000000000000000000 ) ) ;
#20145 = CARTESIAN_POINT ( 'NONE',  ( 10.00000000000000000, 17.83210509884640871, 21.83428559348767806 ) ) ;
#20146 = DIRECTION ( 'NONE',  ( 1.000000000000000000, -0.000000000000000000, -0.000000000000000000 ) ) ;
#20147 = DIRECTION ( 'NONE',  ( -1.000000000000000000, 0.000000000000000000, 0.000000000000000000 ) ) ;
#20148 = CARTESIAN_POINT ( 'NONE',  ( -10.49999999999999822, 0.000000000000000000, 0.000000000000000000 ) ) ;
#20149 = EDGE_CURVE ( 'NONE', #7036, #19371, #20764, .T. ) ;
#20150 = DIRECTION ( 'NONE',  ( 1.000000000000000000, 0.000000000000000000, 0.000000000000000000 ) ) ;
#20151 = ORIENTED_EDGE ( 'NONE', *, *, #957, .T. ) ;
#20152 = EDGE_CURVE ( 'NONE', #14408, #3061, #11601, .T. ) ;
#20153 = LINE ( 'NONE', #18286, #8402 ) ;
#20154 = LINE ( 'NONE', #9970, #16936 ) ;
#20155 = ORIENTED_EDGE ( 'NONE', *, *, #15673, .T. ) ;
#20156 = VECTOR ( 'NONE', #14968, 1000.000000000000000 ) ;
#20157 = CARTESIAN_POINT ( 'NONE',  ( 0.000000000000000000, -56.35896156214997887, 73.34918167666290856 ) ) ;
#20158 = ORIENTED_EDGE ( 'NONE', *, *, #9430, .F. ) ;
#20159 = ORIENTED_EDGE ( 'NONE', *, *, #6269, .T. ) ;
#20160 = DIRECTION ( 'NONE',  ( 0.000000000000000000, 0.2079116908177531808, 0.9781476007338069101 ) ) ;
#20161 = EDGE_CURVE ( 'NONE', #1536, #14184, #8311, .T. ) ;
#20162 = EDGE_LOOP ( 'NONE', ( #8547, #9417, #4377, #10506 ) ) ;
#20163 = ORIENTED_EDGE ( 'NONE', *, *, #4056, .F. ) ;
#20164 = DIRECTION ( 'NONE',  ( 1.000000000000000000, 0.000000000000000000, -0.000000000000000000 ) ) ;
#20165 = CARTESIAN_POINT ( 'NONE',  ( -10.00000000000000000, 0.000000000000000000, 0.000000000000000000 ) ) ;
#20166 = VERTEX_POINT ( 'NONE', #11726 ) ;
#20167 = LINE ( 'NONE', #11873, #16391 ) ;
#20168 = LINE ( 'NONE', #5027, #11879 ) ;
#20169 = CYLINDRICAL_SURFACE ( 'NONE', #3731, 88.00000000000000000 ) ;
#20170 = DIRECTION ( 'NONE',  ( -1.000000000000000000, 0.000000000000000000, 0.000000000000000000 ) ) ;
#20171 = LINE ( 'NONE', #17297, #479 ) ;
#20172 = DIRECTION ( 'NONE',  ( 0.000000000000000000, 0.000000000000000000, -1.000000000000000000 ) ) ;
#20173 = ADVANCED_FACE ( 'NONE', ( #18474 ), #21345, .F. ) ;
#20174 = VERTEX_POINT ( 'NONE', #3552 ) ;
#20175 = EDGE_CURVE ( 'NONE', #13650, #18608, #20075, .T. ) ;
#20176 = DIRECTION ( 'NONE',  ( 1.000000000000000000, 0.000000000000000000, 0.000000000000000000 ) ) ;
#20177 = CARTESIAN_POINT ( 'NONE',  ( 0.000000000000000000, 84.19736439813857487, -38.30455363800847124 ) ) ;
#20178 = ORIENTED_EDGE ( 'NONE', *, *, #12935, .F. ) ;
#20179 =( GEOMETRIC_REPRESENTATION_CONTEXT ( 3 ) GLOBAL_UNCERTAINTY_ASSIGNED_CONTEXT ( ( #9658 ) ) GLOBAL_UNIT_ASSIGNED_CONTEXT ( ( #10091, #13514, #9975 ) ) REPRESENTATION_CONTEXT ( 'NONE', 'WORKASPACE' ) );
#20180 = ADVANCED_FACE ( 'NONE', ( #125 ), #6875, .F. ) ;
#20181 = EDGE_CURVE ( 'NONE', #13328, #19013, #10176, .T. ) ;
#20182 = CARTESIAN_POINT ( 'NONE',  ( -7.600000000000002309, 1.408348717606652665E-14, 114.9007999999999896 ) ) ;
#20183 = EDGE_LOOP ( 'NONE', ( #8607, #14013, #16505, #11513 ) ) ;
#20184 = DIRECTION ( 'NONE',  ( -1.000000000000000000, -0.000000000000000000, -0.000000000000000000 ) ) ;
#20185 = FACE_OUTER_BOUND ( 'NONE', #9948, .T. ) ;
#20186 = ORIENTED_EDGE ( 'NONE', *, *, #15032, .T. ) ;
#20187 = DIRECTION ( 'NONE',  ( 0.000000000000000000, 0.000000000000000000, 1.000000000000000000 ) ) ;
#20188 = AXIS2_PLACEMENT_3D ( 'NONE', #10132, #13447, #1423 ) ;
#20189 = ORIENTED_EDGE ( 'NONE', *, *, #9175, .F. ) ;
#20190 = ORIENTED_EDGE ( 'NONE', *, *, #1537, .T. ) ;
#20191 = VERTEX_POINT ( 'NONE', #1680 ) ;
#20192 = CARTESIAN_POINT ( 'NONE',  ( 10.00000000000000000, 0.000000000000000000, 0.000000000000000000 ) ) ;
#20193 = ORIENTED_EDGE ( 'NONE', *, *, #11511, .F. ) ;
#20194 = CARTESIAN_POINT ( 'NONE',  ( 10.00000000000000000, 0.000000000000000000, 0.000000000000000000 ) ) ;
#20195 = CARTESIAN_POINT ( 'NONE',  ( -10.00000000000000000, 0.000000000000000000, 0.000000000000000000 ) ) ;
#20196 = LINE ( 'NONE', #18542, #5770 ) ;
#20197 = DIRECTION ( 'NONE',  ( 0.000000000000000000, 0.000000000000000000, -1.000000000000000000 ) ) ;
#20198 = CARTESIAN_POINT ( 'NONE',  ( 0.000000000000000000, -15.25521607131222268, 23.70650506194164464 ) ) ;
#20199 = AXIS2_PLACEMENT_3D ( 'NONE', #18917, #12167, #245 ) ;
#20200 = DIRECTION ( 'NONE',  ( -1.000000000000000000, -0.000000000000000000, -0.000000000000000000 ) ) ;
#20201 = CARTESIAN_POINT ( 'NONE',  ( -7.395800000000001262, 0.000000000000000000, 0.000000000000000000 ) ) ;
#20202 = CARTESIAN_POINT ( 'NONE',  ( 0.000000000000000000, 92.49798535263880694, -0.7467976319023919007 ) ) ;
#20203 = CIRCLE ( 'NONE', #6442, 92.50099999999999056 ) ;
#20204 = FACE_OUTER_BOUND ( 'NONE', #10124, .T. ) ;
#20205 = VECTOR ( 'NONE', #13882, 1000.000000000000000 ) ;
#20206 = CARTESIAN_POINT ( 'NONE',  ( 0.000000000000000000, 0.000000000000000000, 0.000000000000000000 ) ) ;
#20207 = VERTEX_POINT ( 'NONE', #15148 ) ;
#20208 = DIRECTION ( 'NONE',  ( 0.000000000000000000, -0.7431448254773861395, -0.6691306063588670083 ) ) ;
#20209 = ORIENTED_EDGE ( 'NONE', *, *, #19542, .T. ) ;
#20210 = DIRECTION ( 'NONE',  ( -1.000000000000000000, 0.000000000000000000, -0.000000000000000000 ) ) ;
#20211 = VERTEX_POINT ( 'NONE', #13483 ) ;
#20212 = CIRCLE ( 'NONE', #13861, 11.99999999999999822 ) ;
#20213 = VERTEX_POINT ( 'NONE', #10182 ) ;
#20214 = ORIENTED_EDGE ( 'NONE', *, *, #10361, .T. ) ;
#20215 = DIRECTION ( 'NONE',  ( -1.000000000000000000, 0.000000000000000000, 0.000000000000000000 ) ) ;
#20216 = AXIS2_PLACEMENT_3D ( 'NONE', #20005, #11822, #16913 ) ;
#20217 = CIRCLE ( 'NONE', #13151, 44.99999999999999289 ) ;
#20218 = ORIENTED_EDGE ( 'NONE', *, *, #2283, .F. ) ;
#20219 = DIRECTION ( 'NONE',  ( 0.000000000000000000, 0.8660254037844398178, -0.4999999999999978351 ) ) ;
#20220 = CARTESIAN_POINT ( 'NONE',  ( 0.000000000000000000, -41.87002153499058466, -74.04114219178087808 ) ) ;
#20221 = VECTOR ( 'NONE', #21632, 1000.000000000000000 ) ;
#20222 = CARTESIAN_POINT ( 'NONE',  ( 10.00000000000000000, 23.57863763525741874, -15.45211464167639548 ) ) ;
#20223 = DIRECTION ( 'NONE',  ( 0.000000000000000000, 0.000000000000000000, 1.000000000000000000 ) ) ;
#20224 = CARTESIAN_POINT ( 'NONE',  ( 5.000000000000002665, -85.54350296776125617, 20.64725405482824883 ) ) ;
#20225 = DIRECTION ( 'NONE',  ( -1.000000000000000000, -0.000000000000000000, 0.000000000000000000 ) ) ;
#20226 = LINE ( 'NONE', #15574, #16172 ) ;
#20227 =( GEOMETRIC_REPRESENTATION_CONTEXT ( 3 ) GLOBAL_UNCERTAINTY_ASSIGNED_CONTEXT ( ( #3051 ) ) GLOBAL_UNIT_ASSIGNED_CONTEXT ( ( #12039, #10369, #4401 ) ) REPRESENTATION_CONTEXT ( 'NONE', 'WORKASPACE' ) );
#20228 = EDGE_CURVE ( 'NONE', #10261, #8175, #18662, .T. ) ;
#20229 = EDGE_LOOP ( 'NONE', ( #15313, #15282, #4656, #8849 ) ) ;
#20230 = CARTESIAN_POINT ( 'NONE',  ( 0.000000000000000000, -27.26034713664101972, 7.182859710736059888 ) ) ;
#20231 = CIRCLE ( 'NONE', #13516, 103.6249999999999716 ) ;
#20232 = AXIS2_PLACEMENT_3D ( 'NONE', #3184, #20092, #6735 ) ;
#20233 = ORIENTED_EDGE ( 'NONE', *, *, #10919, .F. ) ;
#20234 = EDGE_CURVE ( 'NONE', #18952, #10029, #13343, .T. ) ;
#20235 = CIRCLE ( 'NONE', #9262, 32.00000000000000000 ) ;
#20236 = ORIENTED_EDGE ( 'NONE', *, *, #18393, .T. ) ;
#20237 = DIRECTION ( 'NONE',  ( 0.000000000000000000, 0.4067366430758008744, -0.9135454576426006446 ) ) ;
#20238 = AXIS2_PLACEMENT_3D ( 'NONE', #11640, #16705, #7882 ) ;
#20239 = ORIENTED_EDGE ( 'NONE', *, *, #20284, .T. ) ;
#20240 = CARTESIAN_POINT ( 'NONE',  ( -1.139999999999998570, 0.000000000000000000, -6.866799999999992465 ) ) ;
#20241 = VERTEX_POINT ( 'NONE', #20240 ) ;
#20242 = ORIENTED_EDGE ( 'NONE', *, *, #12020, .T. ) ;
#20243 = DIRECTION ( 'NONE',  ( 1.000000000000000000, 0.000000000000000000, 0.000000000000000000 ) ) ;
#20244 = CIRCLE ( 'NONE', #17432, 115.1000000000000227 ) ;
#20245 = EDGE_LOOP ( 'NONE', ( #17788, #6923, #15974, #10241 ) ) ;
#20246 = CARTESIAN_POINT ( 'NONE',  ( 0.000000000000000000, 74.74361964203228581, 40.60271866773572214 ) ) ;
#20247 = VECTOR ( 'NONE', #10752, 1000.000000000000000 ) ;
#20248 = CARTESIAN_POINT ( 'NONE',  ( 10.00000000000000000, -33.95793648385753727, -86.04239391578025220 ) ) ;
#20249 = CYLINDRICAL_SURFACE ( 'NONE', #19533, 44.99999999999999289 ) ;
#20250 = CARTESIAN_POINT ( 'NONE',  ( 5.000000000000000000, 60.65279801375342572, 63.75921967137637836 ) ) ;
#20251 = CIRCLE ( 'NONE', #10713, 44.99999999999999289 ) ;
#20252 = CARTESIAN_POINT ( 'NONE',  ( 1.500000000000000000, 0.000000000000000000, 15.00000000000000000 ) ) ;
#20253 = CYLINDRICAL_SURFACE ( 'NONE', #20984, 115.1000000000000227 ) ;
#20254 = DIRECTION ( 'NONE',  ( 0.000000000000000000, 0.000000000000000000, 1.000000000000000000 ) ) ;
#20255 = ADVANCED_FACE ( 'NONE', ( #11954 ), #24, .T. ) ;
#20256 = EDGE_CURVE ( 'NONE', #6428, #11431, #8598, .T. ) ;
#20257 = ORIENTED_EDGE ( 'NONE', *, *, #1265, .F. ) ;
#20258 = ADVANCED_FACE ( 'NONE', ( #5396 ), #13456, .F. ) ;
#20259 = AXIS2_PLACEMENT_3D ( 'NONE', #3835, #10574, #17321 ) ;
#20260 = DIRECTION ( 'NONE',  ( -1.000000000000000000, 0.000000000000000000, 0.000000000000000000 ) ) ;
#20261 = CIRCLE ( 'NONE', #10724, 11.99999999999999822 ) ;
#20262 = CARTESIAN_POINT ( 'NONE',  ( 0.000000000000000000, 72.58367602204255320, -49.75550195834793499 ) ) ;
#20263 = ORIENTED_EDGE ( 'NONE', *, *, #12600, .F. ) ;
#20264 = DIRECTION ( 'NONE',  ( 0.000000000000000000, 0.000000000000000000, 1.000000000000000000 ) ) ;
#20265 = ORIENTED_EDGE ( 'NONE', *, *, #2882, .F. ) ;
#20266 = AXIS2_PLACEMENT_3D ( 'NONE', #7796, #1389, #19616 ) ;
#20267 = PRESENTATION_STYLE_ASSIGNMENT (( #1811 ) ) ;
#20268 = EDGE_CURVE ( 'NONE', #20166, #9696, #15447, .T. ) ;
#20269 = ORIENTED_EDGE ( 'NONE', *, *, #1503, .F. ) ;
#20270 = CARTESIAN_POINT ( 'NONE',  ( 10.00000000000000000, -84.80486432185219314, 36.94008646920367056 ) ) ;
#20271 = VERTEX_POINT ( 'NONE', #15219 ) ;
#20272 = ORIENTED_EDGE ( 'NONE', *, *, #19845, .F. ) ;
#20273 = CARTESIAN_POINT ( 'NONE',  ( 0.000000000000000000, 0.000000000000000000, -3.000000000000000000 ) ) ;
#20274 = CARTESIAN_POINT ( 'NONE',  ( 10.00000000000000000, 78.83848282823907994, 48.38314403117527718 ) ) ;
#20275 = VERTEX_POINT ( 'NONE', #15330 ) ;
#20276 = EDGE_CURVE ( 'NONE', #3553, #4094, #12027, .T. ) ;
#20277 = DIRECTION ( 'NONE',  ( 1.000000000000000000, 0.000000000000000000, 0.000000000000000000 ) ) ;
#20278 = DIRECTION ( 'NONE',  ( 0.000000000000000000, -0.5877852522924797984, 0.8090169943749425663 ) ) ;
#20279 = DIRECTION ( 'NONE',  ( 0.000000000000000000, 0.4067366430757946572, 0.9135454576426033091 ) ) ;
#20280 = DIRECTION ( 'NONE',  ( -1.000000000000000000, 0.000000000000000000, -0.000000000000000000 ) ) ;
#20281 = DIRECTION ( 'NONE',  ( 0.000000000000000000, 0.000000000000000000, 1.000000000000000000 ) ) ;
#20282 = CARTESIAN_POINT ( 'NONE',  ( 1.500000000000001332, 8.239576745513314221E-16, 6.728125000000023448 ) ) ;
#20283 = AXIS2_PLACEMENT_3D ( 'NONE', #8977, #16046, #2471 ) ;
#20284 = EDGE_CURVE ( 'NONE', #845, #18327, #1365, .T. ) ;
#20285 = ORIENTED_EDGE ( 'NONE', *, *, #1939, .T. ) ;
#20286 = AXIS2_PLACEMENT_3D ( 'NONE', #14506, #12837, #16270 ) ;
#20287 = LINE ( 'NONE', #18632, #18567 ) ;
#20288 = EDGE_CURVE ( 'NONE', #16240, #9108, #13713, .T. ) ;
#20289 = FACE_OUTER_BOUND ( 'NONE', #13190, .T. ) ;
#20290 = ORIENTED_EDGE ( 'NONE', *, *, #4405, .F. ) ;
#20291 = CYLINDRICAL_SURFACE ( 'NONE', #18280, 44.99999999999999289 ) ;
#20292 = VERTEX_POINT ( 'NONE', #4966 ) ;
#20293 = AXIS2_PLACEMENT_3D ( 'NONE', #14130, #10701, #9043 ) ;
#20294 = LINE ( 'NONE', #15089, #17631 ) ;
#20295 = CIRCLE ( 'NONE', #5468, 7.500000000000000000 ) ;
#20296 = DIRECTION ( 'NONE',  ( 0.000000000000000000, 0.000000000000000000, -1.000000000000000000 ) ) ;
#20297 = ORIENTED_EDGE ( 'NONE', *, *, #11108, .F. ) ;
#20298 = CIRCLE ( 'NONE', #11155, 88.00000000000000000 ) ;
#20299 = CARTESIAN_POINT ( 'NONE',  ( 0.000000000000000000, -30.71797041605752554, -82.46457599186584275 ) ) ;
#20300 = EDGE_CURVE ( 'NONE', #20799, #3466, #18679, .T. ) ;
#20301 = AXIS2_PLACEMENT_3D ( 'NONE', #20682, #17587, #5545 ) ;
#20302 = ORIENTED_EDGE ( 'NONE', *, *, #3673, .T. ) ;
#20303 = ORIENTED_EDGE ( 'NONE', *, *, #9027, .T. ) ;
#20304 = VERTEX_POINT ( 'NONE', #18345 ) ;
#20305 = CARTESIAN_POINT ( 'NONE',  ( -10.00000000000000000, 0.000000000000000000, 0.000000000000000000 ) ) ;
#20306 = EDGE_CURVE ( 'NONE', #1, #15334, #2093, .T. ) ;
#20307 = AXIS2_PLACEMENT_3D ( 'NONE', #12136, #3748, #10480 ) ;
#20308 = EDGE_LOOP ( 'NONE', ( #158, #10335, #12175, #8154 ) ) ;
#20309 = CARTESIAN_POINT ( 'NONE',  ( 10.00000000000000000, -75.87763420127865288, 44.57111876559696384 ) ) ;
#20310 = CARTESIAN_POINT ( 'NONE',  ( 10.00000000000000000, -21.65267340503310223, 89.93106657554424999 ) ) ;
#20311 = LINE ( 'NONE', #1741, #9260 ) ;
#20312 = CARTESIAN_POINT ( 'NONE',  ( 10.00000000000000000, 0.000000000000000000, 0.000000000000000000 ) ) ;
#20313 = DIRECTION ( 'NONE',  ( 1.000000000000000000, -0.000000000000000000, -0.000000000000000000 ) ) ;
#20314 = ADVANCED_FACE ( 'NONE', ( #16897 ), #1531, .F. ) ;
#20315 = CIRCLE ( 'NONE', #4416, 92.50100000000000477 ) ;
#20316 = CARTESIAN_POINT ( 'NONE',  ( 10.00000000000000000, 0.000000000000000000, 0.000000000000000000 ) ) ;
#20317 = CIRCLE ( 'NONE', #2303, 12.00000000000000000 ) ;
#20318 = DIRECTION ( 'NONE',  ( 1.000000000000000000, 0.000000000000000000, 0.000000000000000000 ) ) ;
#20319 = CARTESIAN_POINT ( 'NONE',  ( 0.000000000000000000, -80.18694381077126820, 28.37681241246628616 ) ) ;
#20320 = CIRCLE ( 'NONE', #16424, 44.99999999999999289 ) ;
#20321 = EDGE_CURVE ( 'NONE', #18240, #17767, #10256, .T. ) ;
#20322 = LINE ( 'NONE', #20432, #11486 ) ;
#20323 = CARTESIAN_POINT ( 'NONE',  ( -90.00000000000000000, 0.000000000000000000, 0.000000000000000000 ) ) ;
#20324 = ORIENTED_EDGE ( 'NONE', *, *, #17422, .T. ) ;
#20325 = EDGE_LOOP ( 'NONE', ( #7381, #21466, #4513, #2277 ) ) ;
#20326 = CLOSED_SHELL ( 'NONE', ( #16364, #10033, #19349, #40, #16428, #465, #20830, #18083, #10545, #8645, #17564, #17601, #10660, #8169, #6139, #14134, #12345, #11242, #955, #20420, #15025, #21661, #2842, #6811, #3135, #15151, #2656, #4643, #3761, #3546, #11500, #12414, #1485, #12292, #3735, #4519, #4191, #1809, #13536, #10597, #7804, #20465, #8254, #19160 ) ) ;
#20327 = CARTESIAN_POINT ( 'NONE',  ( 0.000000000000000000, 45.60224695560570041, 80.47900393021744492 ) ) ;
#20328 = ORIENTED_EDGE ( 'NONE', *, *, #3097, .F. ) ;
#20329 = CIRCLE ( 'NONE', #7964, 45.00000000000000000 ) ;
#20330 = VERTEX_POINT ( 'NONE', #6847 ) ;
#20331 = AXIS2_PLACEMENT_3D ( 'NONE', #8470, #4115, #8677 ) ;
#20332 = VECTOR ( 'NONE', #14623, 1000.000000000000000 ) ;
#20333 = CIRCLE ( 'NONE', #21014, 103.6250000000000284 ) ;
#20334 = ORIENTED_EDGE ( 'NONE', *, *, #11842, .T. ) ;
#20335 = CIRCLE ( 'NONE', #1276, 44.99999999999999289 ) ;
#20336 = DIRECTION ( 'NONE',  ( -1.000000000000000000, 0.000000000000000000, 0.000000000000000000 ) ) ;
#20337 = ORIENTED_EDGE ( 'NONE', *, *, #7863, .T. ) ;
#20338 = CARTESIAN_POINT ( 'NONE',  ( 10.00000000000000000, 0.000000000000000000, 0.000000000000000000 ) ) ;
#20339 = MANIFOLD_SOLID_BREP ( 'InnerRace', #11137 ) ;
#20340 = CARTESIAN_POINT ( 'NONE',  ( 10.00000000000000000, 0.000000000000000000, 0.000000000000000000 ) ) ;
#20341 = EDGE_CURVE ( 'NONE', #10257, #19369, #17960, .T. ) ;
#20342 = CYLINDRICAL_SURFACE ( 'NONE', #15612, 27.49900000000000233 ) ;
#20343 = FACE_OUTER_BOUND ( 'NONE', #17640, .T. ) ;
#20344 = DIRECTION ( 'NONE',  ( 1.000000000000000000, 0.000000000000000000, 0.000000000000000000 ) ) ;
#20345 = DIRECTION ( 'NONE',  ( 1.000000000000000000, 0.000000000000000000, 0.000000000000000000 ) ) ;
#20346 = CYLINDRICAL_SURFACE ( 'NONE', #9473, 44.99999999999998579 ) ;
#20347 = AXIS2_PLACEMENT_3D ( 'NONE', #3973, #10708, #8735 ) ;
#20348 = ORIENTED_EDGE ( 'NONE', *, *, #18949, .T. ) ;
#20349 = CIRCLE ( 'NONE', #3404, 92.50100000000001899 ) ;
#20350 = CARTESIAN_POINT ( 'NONE',  ( 0.000000000000000000, 87.58454185039451545, -8.540961822680756654 ) ) ;
#20351 = ORIENTED_EDGE ( 'NONE', *, *, #10867, .T. ) ;
#20352 = ORIENTED_EDGE ( 'NONE', *, *, #10758, .T. ) ;
#20353 = CARTESIAN_POINT ( 'NONE',  ( 0.000000000000000000, -23.57863763525731216, 15.45211464167656601 ) ) ;
#20354 = ORIENTED_EDGE ( 'NONE', *, *, #2741, .T. ) ;
#20355 = DIRECTION ( 'NONE',  ( 0.000000000000000000, 0.000000000000000000, -1.000000000000000000 ) ) ;
#20356 = ORIENTED_EDGE ( 'NONE', *, *, #5553, .F. ) ;
#20357 = ORIENTED_EDGE ( 'NONE', *, *, #17195, .T. ) ;
#20358 = EDGE_CURVE ( 'NONE', #5649, #1433, #7033, .T. ) ;
#20359 = DIRECTION ( 'NONE',  ( 1.000000000000000000, 0.000000000000000000, 0.000000000000000000 ) ) ;
#20360 = VERTEX_POINT ( 'NONE', #3738 ) ;
#20361 = AXIS2_PLACEMENT_3D ( 'NONE', #11917, #18667, #8817 ) ;
#20362 = CIRCLE ( 'NONE', #19992, 92.50100000000000477 ) ;
#20363 = CARTESIAN_POINT ( 'NONE',  ( 0.000000000000000000, -35.34277389771475697, -85.48288328206420772 ) ) ;
#20364 = CARTESIAN_POINT ( 'NONE',  ( 10.00000000000000000, -70.37753541435900217, -60.02863908169706519 ) ) ;
#20365 = DIRECTION ( 'NONE',  ( 0.000000000000000000, 0.000000000000000000, 1.000000000000000000 ) ) ;
#20366 = DIRECTION ( 'NONE',  ( 1.000000000000000000, 0.000000000000000000, -0.000000000000000000 ) ) ;
#20367 = EDGE_CURVE ( 'NONE', #5777, #13297, #19093, .T. ) ;
#20368 = DIRECTION ( 'NONE',  ( 1.000000000000000000, 0.000000000000000000, -0.000000000000000000 ) ) ;
#20369 = DIRECTION ( 'NONE',  ( 0.000000000000000000, 0.000000000000000000, -1.000000000000000000 ) ) ;
#20370 = CARTESIAN_POINT ( 'NONE',  ( 0.000000000000000000, -46.93287725819731548, -70.94007663282492615 ) ) ;
#20371 = VERTEX_POINT ( 'NONE', #5506 ) ;
#20372 = CIRCLE ( 'NONE', #16830, 104.9000000000000341 ) ;
#20373 = CIRCLE ( 'NONE', #3082, 88.00000000000000000 ) ;
#20374 = CIRCLE ( 'NONE', #16488, 92.50100000000000477 ) ;
#20375 = FACE_OUTER_BOUND ( 'NONE', #9491, .T. ) ;
#20376 = DIRECTION ( 'NONE',  ( -1.000000000000000000, -0.000000000000000000, -0.000000000000000000 ) ) ;
#20377 = ORIENTED_EDGE ( 'NONE', *, *, #5792, .F. ) ;
#20378 = CARTESIAN_POINT ( 'NONE',  ( 0.000000000000000000, 39.87723064937233630, -83.46401306393528330 ) ) ;
#20379 = ORIENTED_EDGE ( 'NONE', *, *, #2046, .F. ) ;
#20380 = EDGE_LOOP ( 'NONE', ( #10775, #8863, #17202, #17003 ) ) ;
#20381 = CARTESIAN_POINT ( 'NONE',  ( 0.000000000000000000, 81.83745710415276164, 32.35167097270178260 ) ) ;
#20382 = ORIENTED_EDGE ( 'NONE', *, *, #18669, .T. ) ;
#20383 = EDGE_CURVE ( 'NONE', #2563, #739, #12237, .T. ) ;
#20384 = EDGE_LOOP ( 'NONE', ( #10960, #18636, #15891, #1998 ) ) ;
#20385 = CARTESIAN_POINT ( 'NONE',  ( 0.000000000000000000, 0.000000000000000000, 0.000000000000000000 ) ) ;
#20386 = DIRECTION ( 'NONE',  ( 0.000000000000000000, 1.224646799147343593E-16, 1.000000000000000000 ) ) ;
#20387 = DIRECTION ( 'NONE',  ( -1.000000000000000000, 0.000000000000000000, 0.000000000000000000 ) ) ;
#20388 = FACE_OUTER_BOUND ( 'NONE', #1630, .T. ) ;
#20389 = AXIS2_PLACEMENT_3D ( 'NONE', #5479, #17079, #7131 ) ;
#20390 = DIRECTION ( 'NONE',  ( 1.000000000000000000, 0.000000000000000000, 0.000000000000000000 ) ) ;
#20391 = AXIS2_PLACEMENT_3D ( 'NONE', #10977, #2576, #11196 ) ;
#20392 = FACE_OUTER_BOUND ( 'NONE', #19115, .T. ) ;
#20393 = VECTOR ( 'NONE', #922, 1000.000000000000000 ) ;
#20394 = ADVANCED_FACE ( 'NONE', ( #2182 ), #7161, .F. ) ;
#20395 = FACE_OUTER_BOUND ( 'NONE', #12216, .T. ) ;
#20396 = DIRECTION ( 'NONE',  ( 0.000000000000000000, 0.000000000000000000, 1.000000000000000000 ) ) ;
#20397 = ORIENTED_EDGE ( 'NONE', *, *, #20152, .T. ) ;
#20398 = FACE_OUTER_BOUND ( 'NONE', #9227, .T. ) ;
#20399 = ADVANCED_FACE ( 'NONE', ( #10471 ), #13892, .F. ) ;
#20400 = CARTESIAN_POINT ( 'NONE',  ( 10.00000000000000000, -1.592605004252988898, 28.14575649959894221 ) ) ;
#20401 = ORIENTED_EDGE ( 'NONE', *, *, #13794, .F. ) ;
#20402 = DIRECTION ( 'NONE',  ( 1.000000000000000000, 0.000000000000000000, 0.000000000000000000 ) ) ;
#20403 = ORIENTED_EDGE ( 'NONE', *, *, #16100, .T. ) ;
#20404 = CIRCLE ( 'NONE', #17577, 88.00000000000000000 ) ;
#20405 = AXIS2_PLACEMENT_3D ( 'NONE', #1251, #1573, #18384 ) ;
#20406 = FACE_OUTER_BOUND ( 'NONE', #2738, .T. ) ;
#20407 = AXIS2_PLACEMENT_3D ( 'NONE', #18174, #1151, #11419 ) ;
#20408 = VECTOR ( 'NONE', #58, 1000.000000000000000 ) ;
#20409 = FACE_OUTER_BOUND ( 'NONE', #11208, .T. ) ;
#20410 = ORIENTED_EDGE ( 'NONE', *, *, #4064, .T. ) ;
#20412 = EDGE_CURVE ( 'NONE', #8121, #15908, #3140, .T. ) ;
#20411 = ORIENTED_EDGE ( 'NONE', *, *, #20677, .T. ) ;
#20413 = VERTEX_POINT ( 'NONE', #14003 ) ;
#20414 = EDGE_CURVE ( 'NONE', #7194, #15275, #3849, .T. ) ;
#20415 = EDGE_LOOP ( 'NONE', ( #4537, #6146, #13842, #11088 ) ) ;
#20416 = EDGE_CURVE ( 'NONE', #7792, #17973, #20637, .T. ) ;
#20417 = CARTESIAN_POINT ( 'NONE',  ( 0.000000000000000000, -27.00677879429080974, 80.65868421664423238 ) ) ;
#20418 = VERTEX_POINT ( 'NONE', #3949 ) ;
#20419 = CARTESIAN_POINT ( 'NONE',  ( 10.00000000000000000, -19.07277123396555041, 19.80970465344741882 ) ) ;
#20420 = ADVANCED_FACE ( 'NONE', ( #15982, #20855 ), #5721, .T. ) ;
#20421 = DIRECTION ( 'NONE',  ( -1.000000000000000000, 0.000000000000000000, 0.000000000000000000 ) ) ;
#20422 = CARTESIAN_POINT ( 'NONE',  ( -10.00000000000000000, 0.000000000000000000, 0.000000000000000000 ) ) ;
#20423 = DIRECTION ( 'NONE',  ( -1.000000000000000000, -0.000000000000000000, -0.000000000000000000 ) ) ;
#20424 = DIRECTION ( 'NONE',  ( 0.000000000000000000, -0.9945218953682722907, -0.1045284632676634767 ) ) ;
#20425 = CARTESIAN_POINT ( 'NONE',  ( 5.000000000000000000, -27.40684453873955562, -16.51862198942037097 ) ) ;
#20426 = AXIS2_PLACEMENT_3D ( 'NONE', #10153, #20215, #6427 ) ;
#20427 = CARTESIAN_POINT ( 'NONE',  ( 0.000000000000000000, -45.60224695560514618, -80.47900393021774335 ) ) ;
#20428 = DIRECTION ( 'NONE',  ( -1.000000000000000000, 0.000000000000000000, -0.000000000000000000 ) ) ;
#20429 = VECTOR ( 'NONE', #4989, 1000.000000000000000 ) ;
#20430 = DIRECTION ( 'NONE',  ( 0.000000000000000000, 0.000000000000000000, 1.000000000000000000 ) ) ;
#20431 = EDGE_CURVE ( 'NONE', #13819, #16790, #12660, .T. ) ;
#20432 = CARTESIAN_POINT ( 'NONE',  ( 10.00000000000000000, -15.32665449651862843, -91.22241316115434984 ) ) ;
#20433 = EDGE_CURVE ( 'NONE', #12821, #13720, #7487, .T. ) ;
#20434 = DIRECTION ( 'NONE',  ( -1.000000000000000000, -0.000000000000000000, -0.000000000000000000 ) ) ;
#20435 = VERTEX_POINT ( 'NONE', #7277 ) ;
#20436 = DIRECTION ( 'NONE',  ( 1.000000000000000000, -0.000000000000000000, -0.000000000000000000 ) ) ;
#20437 = VERTEX_POINT ( 'NONE', #847 ) ;
#20438 = DIRECTION ( 'NONE',  ( 0.000000000000000000, 0.9945218953682728458, 0.1045284632676570791 ) ) ;
#20439 = ADVANCED_FACE ( 'NONE', ( #20751 ), #16558, .T. ) ;
#20440 = ORIENTED_EDGE ( 'NONE', *, *, #562, .F. ) ;
#20441 = VECTOR ( 'NONE', #336, 1000.000000000000000 ) ;
#20442 = ORIENTED_EDGE ( 'NONE', *, *, #8946, .F. ) ;
#20443 = AXIS2_PLACEMENT_3D ( 'NONE', #19638, #2616, #4501 ) ;
#20444 = AXIS2_PLACEMENT_3D ( 'NONE', #15470, #17132, #3641 ) ;
#20445 = ORIENTED_EDGE ( 'NONE', *, *, #7355, .T. ) ;
#20446 = DIRECTION ( 'NONE',  ( 0.000000000000000000, -0.1391731009600725710, 0.9902680687415692518 ) ) ;
#20447 = EDGE_CURVE ( 'NONE', #18539, #10503, #12350, .T. ) ;
#20448 = ORIENTED_EDGE ( 'NONE', *, *, #6699, .F. ) ;
#20449 = CYLINDRICAL_SURFACE ( 'NONE', #1158, 45.00000000000000000 ) ;
#20450 = DIRECTION ( 'NONE',  ( 1.000000000000000000, 0.000000000000000000, 0.000000000000000000 ) ) ;
#20451 = DIRECTION ( 'NONE',  ( 0.000000000000000000, 0.000000000000000000, 1.000000000000000000 ) ) ;
#20452 = CARTESIAN_POINT ( 'NONE',  ( 1.199999999999992628, 0.000000000000000000, 0.000000000000000000 ) ) ;
#20453 = CARTESIAN_POINT ( 'NONE',  ( 10.00000000000000000, 0.000000000000000000, 0.000000000000000000 ) ) ;
#20454 = CARTESIAN_POINT ( 'NONE',  ( 10.00000000000000000, -3.786343810537388332, -27.23708136986056161 ) ) ;
#20455 = CARTESIAN_POINT ( 'NONE',  ( 10.00000000000000000, -35.34277389771592226, 85.48288328206373876 ) ) ;
#20456 = CIRCLE ( 'NONE', #9482, 44.99999999999998579 ) ;
#20457 = AXIS2_PLACEMENT_3D ( 'NONE', #1050, #7463, #14189 ) ;
#20458 = AXIS2_PLACEMENT_3D ( 'NONE', #4144, #15529, #14092 ) ;
#20459 = ORIENTED_EDGE ( 'NONE', *, *, #12389, .F. ) ;
#20460 = EDGE_CURVE ( 'NONE', #3440, #5218, #1031, .T. ) ;
#20461 = AXIS2_PLACEMENT_3D ( 'NONE', #11698, #17103, #5293 ) ;
#20462 = DIRECTION ( 'NONE',  ( -0.8432271980573100567, 0.000000000000000000, 0.5375573387615669718 ) ) ;
#20463 = ORIENTED_EDGE ( 'NONE', *, *, #1103, .F. ) ;
#20464 = EDGE_CURVE ( 'NONE', #19773, #301, #5610, .T. ) ;
#20465 = ADVANCED_FACE ( 'NONE', ( #17226 ), #8084, .T. ) ;
#20466 = VERTEX_POINT ( 'NONE', #15886 ) ;
#20467 = CARTESIAN_POINT ( 'NONE',  ( 0.000000000000000000, -62.44821182181044605, -68.23969402963567177 ) ) ;
#20468 = ORIENTED_EDGE ( 'NONE', *, *, #21637, .F. ) ;
#20469 = ORIENTED_EDGE ( 'NONE', *, *, #162, .F. ) ;
#20470 = DIRECTION ( 'NONE',  ( -1.000000000000000000, -0.000000000000000000, -0.000000000000000000 ) ) ;
#20471 = ORIENTED_EDGE ( 'NONE', *, *, #13204, .F. ) ;
#20472 = CIRCLE ( 'NONE', #9502, 88.00000000000000000 ) ;
#20473 = FACE_OUTER_BOUND ( 'NONE', #17786, .T. ) ;
#20474 = CARTESIAN_POINT ( 'NONE',  ( 0.000000000000000000, -17.70753755129023332, -21.03896658273990639 ) ) ;
#20475 = CARTESIAN_POINT ( 'NONE',  ( -140.0000507999999968, 0.000000000000000000, -5.000000000000000000 ) ) ;
#20476 = DIRECTION ( 'NONE',  ( -1.000000000000000000, -0.000000000000000000, -0.000000000000000000 ) ) ;
#20477 = CARTESIAN_POINT ( 'NONE',  ( 0.000000000000000000, -0.6021240089803554518, 31.99433460282944708 ) ) ;
#20478 = DIRECTION ( 'NONE',  ( 0.000000000000000000, 0.4067366430757948792, 0.9135454576426031981 ) ) ;
#20479 = CARTESIAN_POINT ( 'NONE',  ( 10.00000000000000000, 86.66425444033963288, -32.33793443156312009 ) ) ;
#20480 = ORIENTED_EDGE ( 'NONE', *, *, #21127, .T. ) ;
#20481 = AXIS2_PLACEMENT_3D ( 'NONE', #17376, #12183, #1909 ) ;
#20482 = DIRECTION ( 'NONE',  ( -1.000000000000000000, -0.000000000000000000, 0.000000000000000000 ) ) ;
#20483 = CARTESIAN_POINT ( 'NONE',  ( 0.000000000000000000, 0.000000000000000000, 0.000000000000000000 ) ) ;
#20484 = ORIENTED_EDGE ( 'NONE', *, *, #12443, .T. ) ;
#20485 = FACE_OUTER_BOUND ( 'NONE', #19228, .T. ) ;
#20486 = ORIENTED_EDGE ( 'NONE', *, *, #20662, .T. ) ;
#20487 =( NAMED_UNIT ( * ) SI_UNIT ( $, .STERADIAN. ) SOLID_ANGLE_UNIT ( ) );
#20488 = ORIENTED_EDGE ( 'NONE', *, *, #7549, .F. ) ;
#20489 = DIRECTION ( 'NONE',  ( 0.000000000000000000, 0.000000000000000000, -1.000000000000000000 ) ) ;
#20490 = ORIENTED_EDGE ( 'NONE', *, *, #13532, .F. ) ;
#20491 = EDGE_LOOP ( 'NONE', ( #12100, #1211, #13089, #7115, #7047 ) ) ;
#20492 = CARTESIAN_POINT ( 'NONE',  ( 5.000000000000000000, -64.95266917914277371, -59.37298010463037912 ) ) ;
#20493 = CARTESIAN_POINT ( 'NONE',  ( -10.00000000000000000, 0.000000000000000000, 0.000000000000000000 ) ) ;
#20494 = DIRECTION ( 'NONE',  ( -1.000000000000000000, -0.000000000000000000, -0.000000000000000000 ) ) ;
#20495 = CARTESIAN_POINT ( 'NONE',  ( 0.000000000000000000, -83.03980459022467642, -18.42770452393328995 ) ) ;
#20496 = DIRECTION ( 'NONE',  ( 1.000000000000000000, 0.000000000000000000, 0.000000000000000000 ) ) ;
#20497 = AXIS2_PLACEMENT_3D ( 'NONE', #20353, #2001, #17358 ) ;
#20498 = DIRECTION ( 'NONE',  ( 0.000000000000000000, 0.000000000000000000, -1.000000000000000000 ) ) ;
#20499 = LINE ( 'NONE', #18516, #5769 ) ;
#20500 = DIRECTION ( 'NONE',  ( 0.8432271980573223802, 0.000000000000000000, -0.5375573387615476539 ) ) ;
#20501 = ORIENTED_EDGE ( 'NONE', *, *, #19319, .F. ) ;
#20502 = DIRECTION ( 'NONE',  ( 1.000000000000000000, 0.000000000000000000, 0.000000000000000000 ) ) ;
#20503 = DIRECTION ( 'NONE',  ( -1.000000000000000000, -0.000000000000000000, 0.000000000000000000 ) ) ;
#20504 = EDGE_CURVE ( 'NONE', #15756, #2852, #9835, .T. ) ;
#20505 = ORIENTED_EDGE ( 'NONE', *, *, #16100, .F. ) ;
#20506 = CYLINDRICAL_SURFACE ( 'NONE', #17221, 88.00000000000000000 ) ;
#20507 = VERTEX_POINT ( 'NONE', #4274 ) ;
#20508 = CYLINDRICAL_SURFACE ( 'NONE', #1744, 88.00000000000000000 ) ;
#20509 = LINE ( 'NONE', #503, #20792 ) ;
#20510 = ORIENTED_EDGE ( 'NONE', *, *, #2263, .T. ) ;
#20511 = EDGE_CURVE ( 'NONE', #569, #9022, #13373, .T. ) ;
#20512 = CARTESIAN_POINT ( 'NONE',  ( 0.000000000000000000, 19.07277123396541185, 19.80970465344755027 ) ) ;
#20513 = ORIENTED_EDGE ( 'NONE', *, *, #72, .F. ) ;
#20514 = ORIENTED_EDGE ( 'NONE', *, *, #10020, .T. ) ;
#20515 = ORIENTED_EDGE ( 'NONE', *, *, #3887, .F. ) ;
#20516 = DIRECTION ( 'NONE',  ( 0.000000000000000000, 0.000000000000000000, -1.000000000000000000 ) ) ;
#20517 = ORIENTED_EDGE ( 'NONE', *, *, #15293, .T. ) ;
#20518 = DIRECTION ( 'NONE',  ( 0.000000000000000000, 0.5299192642331999048, 0.8480480961564290654 ) ) ;
#20519 = CARTESIAN_POINT ( 'NONE',  ( 10.00000000000000000, 0.000000000000000000, 0.000000000000000000 ) ) ;
#20520 = DIRECTION ( 'NONE',  ( -1.000000000000000000, 0.000000000000000000, 0.000000000000000000 ) ) ;
#20521 = CARTESIAN_POINT ( 'NONE',  ( -90.00000000000000000, 0.000000000000000000, 0.000000000000000000 ) ) ;
#20522 = DIRECTION ( 'NONE',  ( 0.000000000000000000, 0.000000000000000000, 1.000000000000000000 ) ) ;
#20523 = DIRECTION ( 'NONE',  ( 1.000000000000000000, 0.000000000000000000, 0.000000000000000000 ) ) ;
#20524 = CIRCLE ( 'NONE', #13818, 1.100000000000003642 ) ;
#20525 = DIRECTION ( 'NONE',  ( 0.000000000000000000, 0.7880107536067190166, 0.6156614753256620665 ) ) ;
#20526 = DIRECTION ( 'NONE',  ( 1.000000000000000000, 0.000000000000000000, 0.000000000000000000 ) ) ;
#20527 = PRODUCT_DEFINITION_FORMATION_WITH_SPECIFIED_SOURCE ( 'ANY', '', #9642, .NOT_KNOWN. ) ;
#20528 = EDGE_LOOP ( 'NONE', ( #4685, #17259, #21265, #7889 ) ) ;
#20529 = FACE_OUTER_BOUND ( 'NONE', #990, .T. ) ;
#20530 = DIRECTION ( 'NONE',  ( -1.000000000000000000, -0.000000000000000000, 0.000000000000000000 ) ) ;
#20531 = ADVANCED_FACE ( 'NONE', ( #14778, #11130 ), #4387, .T. ) ;
#20532 = EDGE_CURVE ( 'NONE', #14363, #11540, #665, .T. ) ;
#20533 = EDGE_CURVE ( 'NONE', #4414, #19161, #9455, .T. ) ;
#20534 = LINE ( 'NONE', #18766, #12582 ) ;
#20535 = ORIENTED_EDGE ( 'NONE', *, *, #2018, .F. ) ;
#20536 = ADVANCED_FACE ( 'NONE', ( #14879 ), #14441, .F. ) ;
#20537 = DIRECTION ( 'NONE',  ( 1.000000000000000000, 0.000000000000000000, 0.000000000000000000 ) ) ;
#20538 = VERTEX_POINT ( 'NONE', #21519 ) ;
#20539 = DIRECTION ( 'NONE',  ( 1.000000000000000000, 0.000000000000000000, 0.000000000000000000 ) ) ;
#20540 = VERTEX_POINT ( 'NONE', #12890 ) ;
#20541 = ORIENTED_EDGE ( 'NONE', *, *, #3411, .T. ) ;
#20542 = DIRECTION ( 'NONE',  ( 1.000000000000000000, 0.000000000000000000, 0.000000000000000000 ) ) ;
#20543 = VERTEX_POINT ( 'NONE', #16097 ) ;
#20544 = EDGE_CURVE ( 'NONE', #5051, #16474, #5977, .T. ) ;
#20545 = CARTESIAN_POINT ( 'NONE',  ( 10.00000000000000000, 0.000000000000000000, 0.000000000000000000 ) ) ;
#20546 = DIRECTION ( 'NONE',  ( 0.000000000000000000, -0.9945218953682722907, -0.1045284632676636849 ) ) ;
#20547 = DIRECTION ( 'NONE',  ( 1.000000000000000000, 0.000000000000000000, 0.000000000000000000 ) ) ;
#20548 = CARTESIAN_POINT ( 'NONE',  ( 0.000000000000000000, 41.87002153499211232, -74.04114219178001122 ) ) ;
#20549 = ADVANCED_FACE ( 'NONE', ( #7812 ), #13017, .T. ) ;
#20550 = VECTOR ( 'NONE', #4424, 1000.000000000000000 ) ;
#20551 = DIRECTION ( 'NONE',  ( 0.000000000000000000, 0.000000000000000000, 1.000000000000000000 ) ) ;
#20552 = DIRECTION ( 'NONE',  ( 1.000000000000000000, 0.000000000000000000, -0.000000000000000000 ) ) ;
#20553 = PLANE ( 'NONE',  #8625 ) ;
#20554 = DIRECTION ( 'NONE',  ( -0.000000000000000000, -0.000000000000000000, 1.000000000000000000 ) ) ;
#20555 = DIRECTION ( 'NONE',  ( 0.000000000000000000, 0.000000000000000000, 1.000000000000000000 ) ) ;
#20556 = ORIENTED_EDGE ( 'NONE', *, *, #15183, .F. ) ;
#20557 = DIRECTION ( 'NONE',  ( 0.000000000000000000, 0.000000000000000000, 1.000000000000000000 ) ) ;
#20558 = EDGE_CURVE ( 'NONE', #17412, #1609, #9471, .T. ) ;
#20559 = VERTEX_POINT ( 'NONE', #12669 ) ;
#20560 = ORIENTED_EDGE ( 'NONE', *, *, #4449, .T. ) ;
#20561 = DIRECTION ( 'NONE',  ( -1.000000000000000000, -0.000000000000000000, 0.000000000000000000 ) ) ;
#20562 = EDGE_LOOP ( 'NONE', ( #14809, #4155, #4152, #11749 ) ) ;
#20563 = VERTEX_POINT ( 'NONE', #1298 ) ;
#20564 = AXIS2_PLACEMENT_3D ( 'NONE', #20201, #8378, #13451 ) ;
#20565 = ADVANCED_FACE ( 'NONE', ( #11238, #18088 ), #17990, .F. ) ;
#20566 = CARTESIAN_POINT ( 'NONE',  ( 0.000000000000000000, -71.33759994382000968, 58.88447872958963814 ) ) ;
#20567 = VERTEX_POINT ( 'NONE', #21185 ) ;
#20568 = ADVANCED_FACE ( 'NONE', ( #3059 ), #9558, .F. ) ;
#20569 = DIRECTION ( 'NONE',  ( 1.000000000000000000, 0.000000000000000000, 0.000000000000000000 ) ) ;
#20570 = VECTOR ( 'NONE', #652, 1000.000000000000000 ) ;
#20571 = DIRECTION ( 'NONE',  ( 1.000000000000000000, 0.000000000000000000, 0.000000000000000000 ) ) ;
#20572 = CARTESIAN_POINT ( 'NONE',  ( -8.900000000000018119, 0.000000000000000000, -118.9000000000000199 ) ) ;
#20573 = CARTESIAN_POINT ( 'NONE',  ( 5.000000000000000000, -60.65279801375299229, -63.75921967137679047 ) ) ;
#20574 = EDGE_CURVE ( 'NONE', #8180, #3874, #1412, .T. ) ;
#20575 = EDGE_CURVE ( 'NONE', #18927, #19144, #21490, .T. ) ;
#20576 = DIRECTION ( 'NONE',  ( -1.000000000000000000, 0.000000000000000000, 0.000000000000000000 ) ) ;
#20577 = CARTESIAN_POINT ( 'NONE',  ( 1.399999999999999245, 0.000000000000000000, 0.000000000000000000 ) ) ;
#20578 = CARTESIAN_POINT ( 'NONE',  ( 10.00000000000000000, -71.72924546249915068, -45.71766382684744201 ) ) ;
#20579 = EDGE_LOOP ( 'NONE', ( #20690, #16590 ) ) ;
#20580 = AXIS2_PLACEMENT_3D ( 'NONE', #2351, #13956, #8657 ) ;
#20581 = EDGE_CURVE ( 'NONE', #378, #15558, #1180, .T. ) ;
#20582 = DIRECTION ( 'NONE',  ( 0.000000000000000000, 0.000000000000000000, 1.000000000000000000 ) ) ;
#20583 = LINE ( 'NONE', #20903, #15168 ) ;
#20584 = PRESENTATION_LAYER_ASSIGNMENT (  '', '', ( #5421 ) ) ;
#20585 = EDGE_LOOP ( 'NONE', ( #8422, #6062, #15858, #3116 ) ) ;
#20586 = CYLINDRICAL_SURFACE ( 'NONE', #3019, 92.50100000000000477 ) ;
#20587 = ORIENTED_EDGE ( 'NONE', *, *, #11903, .F. ) ;
#20588 = CONICAL_SURFACE ( 'NONE', #18467, 103.6249999999999716, 0.5675376247847775391 ) ;
#20589 = CARTESIAN_POINT ( 'NONE',  ( 10.00000000000000000, 71.33759994381962599, 58.88447872959010709 ) ) ;
#20590 = ORIENTED_EDGE ( 'NONE', *, *, #1044, .T. ) ;
#20591 = ORIENTED_EDGE ( 'NONE', *, *, #2100, .T. ) ;
#20592 = DIRECTION ( 'NONE',  ( 0.000000000000000000, 0.6427876096865353661, 0.7660444431189813441 ) ) ;
#20593 = CARTESIAN_POINT ( 'NONE',  ( 10.00000000000000000, 21.31452625071037943, -82.34610137166097843 ) ) ;
#20594 = AXIS2_PLACEMENT_3D ( 'NONE', #8692, #15426, #10453 ) ;
#20595 = AXIS2_PLACEMENT_3D ( 'NONE', #4570, #3227, #11302 ) ;
#20596 = CARTESIAN_POINT ( 'NONE',  ( -10.00000000000000000, 0.000000000000000000, 0.000000000000000000 ) ) ;
#20597 = DIRECTION ( 'NONE',  ( -1.000000000000000000, 0.000000000000000000, 0.000000000000000000 ) ) ;
#20598 = CARTESIAN_POINT ( 'NONE',  ( -10.00000000000000000, 0.000000000000000000, 0.000000000000000000 ) ) ;
#20599 = CARTESIAN_POINT ( 'NONE',  ( -90.00000000000000000, 0.000000000000000000, 0.000000000000000000 ) ) ;
#20600 = CYLINDRICAL_SURFACE ( 'NONE', #16703, 44.99999999999998579 ) ;
#20601 = CARTESIAN_POINT ( 'NONE',  ( -8.000000000000007105, 0.000000000000000000, -104.9000000000000341 ) ) ;
#20602 = AXIS2_PLACEMENT_3D ( 'NONE', #13195, #21505, #16297 ) ;
#20603 = ORIENTED_EDGE ( 'NONE', *, *, #10407, .T. ) ;
#20604 = DIRECTION ( 'NONE',  ( 1.000000000000000000, 0.000000000000000000, 0.000000000000000000 ) ) ;
#20605 = AXIS2_PLACEMENT_3D ( 'NONE', #12740, #12311, #7452 ) ;
#20606 = ORIENTED_EDGE ( 'NONE', *, *, #17310, .F. ) ;
#20607 = CIRCLE ( 'NONE', #17078, 120.0000000000000000 ) ;
#20608 = CARTESIAN_POINT ( 'NONE',  ( 10.00000000000000000, -83.35585896458628952, 16.94078559807922346 ) ) ;
#20609 = ORIENTED_EDGE ( 'NONE', *, *, #18382, .F. ) ;
#20610 = FACE_BOUND ( 'NONE', #18727, .T. ) ;
#20611 = DIRECTION ( 'NONE',  ( 0.000000000000000000, 0.000000000000000000, 1.000000000000000000 ) ) ;
#20612 = ORIENTED_EDGE ( 'NONE', *, *, #13888, .F. ) ;
#20613 = CIRCLE ( 'NONE', #11087, 44.99999999999999289 ) ;
#20614 = ORIENTED_EDGE ( 'NONE', *, *, #5461, .T. ) ;
#20615 = ORIENTED_EDGE ( 'NONE', *, *, #16079, .F. ) ;
#20616 = VERTEX_POINT ( 'NONE', #9345 ) ;
#20617 = DIRECTION ( 'NONE',  ( 0.000000000000000000, 1.000000000000000000, 0.000000000000000000 ) ) ;
#20618 = VERTEX_POINT ( 'NONE', #14659 ) ;
#20619 = AXIS2_PLACEMENT_3D ( 'NONE', #1060, #11433, #12872 ) ;
#20620 = DIRECTION ( 'NONE',  ( -1.000000000000000000, 0.000000000000000000, 0.000000000000000000 ) ) ;
#20621 = CARTESIAN_POINT ( 'NONE',  ( 10.00000000000000000, 0.000000000000000000, 0.000000000000000000 ) ) ;
#20622 = EDGE_CURVE ( 'NONE', #13868, #17955, #2944, .T. ) ;
#20623 = CYLINDRICAL_SURFACE ( 'NONE', #8644, 12.00000000000000000 ) ;
#20624 = DIRECTION ( 'NONE',  ( -1.000000000000000000, -0.000000000000000000, -0.000000000000000000 ) ) ;
#20625 = CIRCLE ( 'NONE', #18520, 11.99999999999999467 ) ;
#20626 = DIRECTION ( 'NONE',  ( 0.000000000000000000, -0.2079116908177664480, 0.9781476007338041345 ) ) ;
#20627 = CARTESIAN_POINT ( 'NONE',  ( 0.000000000000000000, 0.000000000000000000, 0.000000000000000000 ) ) ;
#20628 = ORIENTED_EDGE ( 'NONE', *, *, #21258, .F. ) ;
#20629 = EDGE_CURVE ( 'NONE', #9563, #8475, #20294, .T. ) ;
#20630 = DIRECTION ( 'NONE',  ( -1.000000000000000000, 0.000000000000000000, 0.000000000000000000 ) ) ;
#20631 = CARTESIAN_POINT ( 'NONE',  ( 0.000000000000000000, 21.69483248597444813, -16.89761061231758177 ) ) ;
#20632 = AXIS2_PLACEMENT_3D ( 'NONE', #11476, #16565, #6629 ) ;
#20633 = VECTOR ( 'NONE', #13008, 1000.000000000000000 ) ;
#20634 = CARTESIAN_POINT ( 'NONE',  ( 10.00000000000000000, 66.01871308925549897, -64.79170103522952218 ) ) ;
#20635 = AXIS2_PLACEMENT_3D ( 'NONE', #2684, #1138, #11190 ) ;
#20636 = VERTEX_POINT ( 'NONE', #14979 ) ;
#20637 = LINE ( 'NONE', #10584, #4548 ) ;
#20638 = ORIENTED_EDGE ( 'NONE', *, *, #9277, .F. ) ;
#20639 = FACE_OUTER_BOUND ( 'NONE', #11918, .T. ) ;
#20640 = AXIS2_PLACEMENT_3D ( 'NONE', #10804, #5848, #5734 ) ;
#20641 = ORIENTED_EDGE ( 'NONE', *, *, #19845, .T. ) ;
#20642 = EDGE_LOOP ( 'NONE', ( #2509, #9591, #10583, #20556, #16572, #7066, #6551, #10567 ) ) ;
#20643 = ORIENTED_EDGE ( 'NONE', *, *, #7, .F. ) ;
#20644 = CARTESIAN_POINT ( 'NONE',  ( 10.00000000000000000, 0.000000000000000000, 0.000000000000000000 ) ) ;
#20645 = DIRECTION ( 'NONE',  ( 1.000000000000000000, 0.000000000000000000, 0.000000000000000000 ) ) ;
#20646 = DIRECTION ( 'NONE',  ( 0.000000000000000000, 0.2079116908177599810, -0.9781476007338055778 ) ) ;
#20647 = EDGE_CURVE ( 'NONE', #12372, #5601, #5268, .T. ) ;
#20648 = AXIS2_PLACEMENT_3D ( 'NONE', #9779, #9897, #18082 ) ;
#20649 = MANIFOLD_SOLID_BREP ( 'Extrude-Thin1', #199 ) ;
#20650 = DIRECTION ( 'NONE',  ( -1.000000000000000000, 0.000000000000000000, 0.000000000000000000 ) ) ;
#20651 = CIRCLE ( 'NONE', #15715, 92.50100000000000477 ) ;
#20652 = PRODUCT_DEFINITION_CONTEXT ( 'detailed design', #18859, 'design' ) ;
#20653 = AXIS2_PLACEMENT_3D ( 'NONE', #3453, #11961, #6680 ) ;
#20654 = DIRECTION ( 'NONE',  ( 0.000000000000000000, -0.1391731009600517821, -0.9902680687415721383 ) ) ;
#20655 = CYLINDRICAL_SURFACE ( 'NONE', #15774, 44.99999999999999289 ) ;
#20656 = CARTESIAN_POINT ( 'NONE',  ( 10.00000000000000000, 0.000000000000000000, 0.000000000000000000 ) ) ;
#20657 = CARTESIAN_POINT ( 'NONE',  ( 10.00000000000000000, 89.12061559554334167, 24.77803214283572686 ) ) ;
#20658 = DIRECTION ( 'NONE',  ( 0.000000000000000000, 0.8660254037844398178, -0.4999999999999978351 ) ) ;
#20659 = CLOSED_SHELL ( 'NONE', ( #20954, #11542, #4037, #15525, #10273, #20805, #334, #12057, #5034, #10442, #14756, #13638, #8282, #12576, #7292, #3278, #8709, #5953, #16893 ) ) ;
#20660 = ORIENTED_EDGE ( 'NONE', *, *, #18958, .F. ) ;
#20661 = CARTESIAN_POINT ( 'NONE',  ( -10.00000000000000000, 0.000000000000000000, 0.000000000000000000 ) ) ;
#20662 = EDGE_CURVE ( 'NONE', #11788, #15688, #8686, .T. ) ;
#20663 = VERTEX_POINT ( 'NONE', #21613 ) ;
#20664 = ORIENTED_EDGE ( 'NONE', *, *, #11483, .T. ) ;
#20665 = CIRCLE ( 'NONE', #9699, 45.00000000000000711 ) ;
#20666 = VECTOR ( 'NONE', #5469, 1000.000000000000000 ) ;
#20667 = ORIENTED_EDGE ( 'NONE', *, *, #19188, .T. ) ;
#20668 = ADVANCED_FACE ( 'NONE', ( #15306 ), #13545, .T. ) ;
#20669 = CIRCLE ( 'NONE', #18907, 44.99999999999998579 ) ;
#20670 = DIRECTION ( 'NONE',  ( 0.000000000000000000, 0.000000000000000000, 1.000000000000000000 ) ) ;
#20671 = ORIENTED_EDGE ( 'NONE', *, *, #13204, .T. ) ;
#20672 = ORIENTED_EDGE ( 'NONE', *, *, #15492, .F. ) ;
#20673 = DIRECTION ( 'NONE',  ( 0.000000000000000000, -0.5877852522924632561, -0.8090169943749546677 ) ) ;
#20674 = EDGE_CURVE ( 'NONE', #2294, #3283, #5995, .T. ) ;
#20675 = ORIENTED_EDGE ( 'NONE', *, *, #4604, .F. ) ;
#20676 = EDGE_CURVE ( 'NONE', #155, #15057, #16920, .T. ) ;
#20677 = EDGE_CURVE ( 'NONE', #11211, #5130, #3511, .T. ) ;
#20678 = DIRECTION ( 'NONE',  ( -1.000000000000000000, -0.000000000000000000, -0.000000000000000000 ) ) ;
#20679 = CARTESIAN_POINT ( 'NONE',  ( 10.00000000000000000, 0.000000000000000000, 1.000000000000000000 ) ) ;
#20680 = VECTOR ( 'NONE', #4903, 1000.000000000000000 ) ;
#20681 = EDGE_CURVE ( 'NONE', #771, #13033, #13740, .T. ) ;
#20682 = CARTESIAN_POINT ( 'NONE',  ( -10.00000000000002309, 0.000000000000000000, 0.000000000000000000 ) ) ;
#20683 = DIRECTION ( 'NONE',  ( -1.000000000000000000, -0.000000000000000000, -0.000000000000000000 ) ) ;
#20684 = AXIS2_PLACEMENT_3D ( 'NONE', #14136, #8620, #10605 ) ;
#20685 = DIRECTION ( 'NONE',  ( 1.000000000000000000, 0.000000000000000000, 0.000000000000000000 ) ) ;
#20686 = CARTESIAN_POINT ( 'NONE',  ( -7.395800000000001262, 1.287093988729475069E-14, 105.0992000000000104 ) ) ;
#20687 = DIRECTION ( 'NONE',  ( 0.000000000000000000, 0.9848077530122085754, -0.1736481776669273613 ) ) ;
#20689 = AXIS2_PLACEMENT_3D ( 'NONE', #6091, #20094, #18335 ) ;
#20688 = CARTESIAN_POINT ( 'NONE',  ( 0.000000000000000000, -52.96496548042809138, -66.55750800669412115 ) ) ;
#20690 = ORIENTED_EDGE ( 'NONE', *, *, #13236, .T. ) ;
#20691 = EDGE_CURVE ( 'NONE', #11544, #17790, #19031, .T. ) ;
#20692 = ADVANCED_FACE ( 'NONE', ( #16975 ), #8572, .F. ) ;
#20693 = DIRECTION ( 'NONE',  ( 0.000000000000000000, 0.000000000000000000, 1.000000000000000000 ) ) ;
#20694 = ADVANCED_FACE ( 'NONE', ( #20406 ), #11998, .F. ) ;
#20695 = CARTESIAN_POINT ( 'NONE',  ( 10.00000000000000000, 73.32282170386913833, -48.65967342042704757 ) ) ;
#20696 = ORIENTED_EDGE ( 'NONE', *, *, #6219, .F. ) ;
#20697 = CIRCLE ( 'NONE', #10473, 44.99999999999999289 ) ;
#20698 = CARTESIAN_POINT ( 'NONE',  ( 10.00000000000000000, 0.000000000000000000, 0.000000000000000000 ) ) ;
#20699 = ORIENTED_EDGE ( 'NONE', *, *, #15011, .F. ) ;
#20700 = AXIS2_PLACEMENT_3D ( 'NONE', #2877, #21441, #18132 ) ;
#20701 = ADVANCED_FACE ( 'NONE', ( #18322 ), #3172, .T. ) ;
#20702 = DIRECTION ( 'NONE',  ( 1.000000000000000000, 0.000000000000000000, 0.000000000000000000 ) ) ;
#20703 = DIRECTION ( 'NONE',  ( 0.000000000000000000, 0.000000000000000000, 1.000000000000000000 ) ) ;
#20704 = ORIENTED_EDGE ( 'NONE', *, *, #6784, .F. ) ;
#20705 = ORIENTED_EDGE ( 'NONE', *, *, #13020, .F. ) ;
#20706 = FACE_OUTER_BOUND ( 'NONE', #21024, .T. ) ;
#20707 = CARTESIAN_POINT ( 'NONE',  ( 0.000000000000000000, -71.72924546249979016, 45.71766382684644725 ) ) ;
#20708 = EDGE_CURVE ( 'NONE', #1355, #20086, #16220, .T. ) ;
#20709 = CARTESIAN_POINT ( 'NONE',  ( 0.000000000000000000, 0.000000000000000000, 0.000000000000000000 ) ) ;
#20710 = DIRECTION ( 'NONE',  ( 0.000000000000000000, 0.2079116908177599532, -0.9781476007338055778 ) ) ;
#20711 = CARTESIAN_POINT ( 'NONE',  ( 10.00000000000000000, 0.000000000000000000, 0.000000000000000000 ) ) ;
#20712 = DIRECTION ( 'NONE',  ( -1.000000000000000000, 0.000000000000000000, -0.000000000000000000 ) ) ;
#20713 = ADVANCED_FACE ( 'NONE', ( #15416 ), #15863, .T. ) ;
#20714 = CYLINDRICAL_SURFACE ( 'NONE', #8940, 88.00000000000000000 ) ;
#20715 = DIRECTION ( 'NONE',  ( 0.000000000000000000, 0.000000000000000000, 1.000000000000000000 ) ) ;
#20716 = CIRCLE ( 'NONE', #15058, 45.00000000000000000 ) ;
#20717 = VERTEX_POINT ( 'NONE', #722 ) ;
#20718 = CIRCLE ( 'NONE', #8369, 6.866799999999992465 ) ;
#20719 = CARTESIAN_POINT ( 'NONE',  ( 0.000000000000000000, -79.38136668499713267, -37.98155635597392887 ) ) ;
#20720 = VERTEX_POINT ( 'NONE', #15747 ) ;
#20721 = EDGE_CURVE ( 'NONE', #18882, #9461, #5368, .T. ) ;
#20722 = DIRECTION ( 'NONE',  ( 0.000000000000000000, 0.000000000000000000, 1.000000000000000000 ) ) ;
#20723 = ORIENTED_EDGE ( 'NONE', *, *, #4323, .F. ) ;
#20724 = CARTESIAN_POINT ( 'NONE',  ( 10.00000000000000000, -24.89070495400676819, -84.40647372620527733 ) ) ;
#20725 = CARTESIAN_POINT ( 'NONE',  ( -7.440711023145607506, 1.409568465818603827E-14, 115.1000000000000227 ) ) ;
#20726 = ORIENTED_EDGE ( 'NONE', *, *, #14777, .F. ) ;
#20727 = ADVANCED_FACE ( 'NONE', ( #5481 ), #20508, .F. ) ;
#20728 = SURFACE_STYLE_FILL_AREA ( #7366 ) ;
#20729 = CIRCLE ( 'NONE', #3092, 11.99999999999999822 ) ;
#20730 = VERTEX_POINT ( 'NONE', #3924 ) ;
#20731 = VERTEX_POINT ( 'NONE', #3705 ) ;
#20732 = AXIS2_PLACEMENT_3D ( 'NONE', #392, #5587, #3815 ) ;
#20733 = VERTEX_POINT ( 'NONE', #12098 ) ;
#20734 = CYLINDRICAL_SURFACE ( 'NONE', #11076, 92.50100000000000477 ) ;
#20735 = EDGE_LOOP ( 'NONE', ( #2433, #12646, #6600, #16009 ) ) ;
#20736 = DIRECTION ( 'NONE',  ( 1.000000000000000000, 0.000000000000000000, 0.000000000000000000 ) ) ;
#20737 = CARTESIAN_POINT ( 'NONE',  ( 10.00000000000000000, 27.26034713664087406, 7.182859710736605230 ) ) ;
#20738 = CARTESIAN_POINT ( 'NONE',  ( 0.000000000000000000, -88.70892494636754577, 26.21376805916555242 ) ) ;
#20739 = CARTESIAN_POINT ( 'NONE',  ( 10.00000000000000000, 27.07404830566971299, 4.815694066514526028 ) ) ;
#20740 = CARTESIAN_POINT ( 'NONE',  ( 10.00000000000000000, -91.70173545986527586, 12.13370160540012499 ) ) ;
#20741 = CYLINDRICAL_SURFACE ( 'NONE', #21271, 88.00000000000000000 ) ;
#20742 = ORIENTED_EDGE ( 'NONE', *, *, #15080, .F. ) ;
#20743 = FACE_OUTER_BOUND ( 'NONE', #18473, .T. ) ;
#20744 = CARTESIAN_POINT ( 'NONE',  ( 8.000000000000007105, 0.000000000000000000, 0.000000000000000000 ) ) ;
#20745 = AXIS2_PLACEMENT_3D ( 'NONE', #14383, #10626, #14497 ) ;
#20746 = AXIS2_PLACEMENT_3D ( 'NONE', #17318, #20520, #5603 ) ;
#20747 = AXIS2_PLACEMENT_3D ( 'NONE', #3132, #9634, #20037 ) ;
#20748 = EDGE_CURVE ( 'NONE', #16515, #11372, #5284, .T. ) ;
#20749 = DIRECTION ( 'NONE',  ( -1.000000000000000000, -0.000000000000000000, -0.000000000000000000 ) ) ;
#20750 = EDGE_LOOP ( 'NONE', ( #19015, #11885, #14385, #8801 ) ) ;
#20751 = FACE_OUTER_BOUND ( 'NONE', #14219, .T. ) ;
#20752 = VERTEX_POINT ( 'NONE', #20724 ) ;
#20753 = DIRECTION ( 'NONE',  ( 0.000000000000000000, 0.000000000000000000, 1.000000000000000000 ) ) ;
#20754 = ORIENTED_EDGE ( 'NONE', *, *, #5535, .T. ) ;
#20755 = CIRCLE ( 'NONE', #18285, 113.8250000000000171 ) ;
#20756 = ORIENTED_EDGE ( 'NONE', *, *, #5684, .T. ) ;
#20757 = ORIENTED_EDGE ( 'NONE', *, *, #17741, .F. ) ;
#20758 = LINE ( 'NONE', #7716, #9723 ) ;
#20759 = ORIENTED_EDGE ( 'NONE', *, *, #16211, .F. ) ;
#20760 = CARTESIAN_POINT ( 'NONE',  ( 10.00000000000000000, 0.000000000000000000, 0.000000000000000000 ) ) ;
#20761 = LINE ( 'NONE', #14125, #1934 ) ;
#20762 = CARTESIAN_POINT ( 'NONE',  ( -140.0000507999999968, 0.000000000000000000, 0.000000000000000000 ) ) ;
#20763 = CIRCLE ( 'NONE', #15825, 92.50100000000000477 ) ;
#20764 = CIRCLE ( 'NONE', #21128, 44.99999999999998579 ) ;
#20765 = CIRCLE ( 'NONE', #8417, 92.50100000000000477 ) ;
#20766 = DIRECTION ( 'NONE',  ( 0.000000000000000000, 0.000000000000000000, -1.000000000000000000 ) ) ;
#20767 = CYLINDRICAL_SURFACE ( 'NONE', #13865, 92.50100000000000477 ) ;
#20768 = DIRECTION ( 'NONE',  ( 0.000000000000000000, 0.9993908270190955401, 0.03489949670250440394 ) ) ;
#20769 = CARTESIAN_POINT ( 'NONE',  ( 10.00000000000000000, 78.04699792498145428, 49.64978465107317618 ) ) ;
#20770 = CYLINDRICAL_SURFACE ( 'NONE', #10843, 3.000000000000000444 ) ;
#20771 = DIRECTION ( 'NONE',  ( -1.000000000000000000, -0.000000000000000000, 0.000000000000000000 ) ) ;
#20772 = VERTEX_POINT ( 'NONE', #7359 ) ;
#20773 = CARTESIAN_POINT ( 'NONE',  ( 5.000000000000002665, -29.47587714450981622, -82.91666097089152743 ) ) ;
#20774 = ORIENTED_EDGE ( 'NONE', *, *, #16609, .T. ) ;
#20775 = EDGE_CURVE ( 'NONE', #18856, #5686, #7754, .T. ) ;
#20776 = AXIS2_PLACEMENT_3D ( 'NONE', #12099, #18962, #17408 ) ;
#20777 = ORIENTED_EDGE ( 'NONE', *, *, #8828, .F. ) ;
#20778 = AXIS2_PLACEMENT_3D ( 'NONE', #3524, #94, #1756 ) ;
#20779 = ORIENTED_EDGE ( 'NONE', *, *, #7937, .T. ) ;
#20780 = CYLINDRICAL_SURFACE ( 'NONE', #18026, 44.99999999999999289 ) ;
#20781 = ORIENTED_EDGE ( 'NONE', *, *, #16943, .F. ) ;
#20782 = ORIENTED_EDGE ( 'NONE', *, *, #16150, .F. ) ;
#20783 = ADVANCED_FACE ( 'NONE', ( #10877 ), #10762, .T. ) ;
#20784 = DIRECTION ( 'NONE',  ( 0.000000000000000000, 0.000000000000000000, 1.000000000000000000 ) ) ;
#20785 = ORIENTED_EDGE ( 'NONE', *, *, #14980, .T. ) ;
#20786 = CARTESIAN_POINT ( 'NONE',  ( -10.00000000000000000, 0.000000000000000000, 0.000000000000000000 ) ) ;
#20787 = CARTESIAN_POINT ( 'NONE',  ( 10.00000000000000000, -17.83210509884626660, -21.83428559348779530 ) ) ;
#20788 = EDGE_CURVE ( 'NONE', #5152, #4275, #19388, .T. ) ;
#20789 = AXIS2_PLACEMENT_3D ( 'NONE', #13778, #8583, #4128 ) ;
#20790 = DIRECTION ( 'NONE',  ( -1.000000000000000000, 0.000000000000000000, 0.000000000000000000 ) ) ;
#20791 = DIRECTION ( 'NONE',  ( -1.000000000000000000, -0.000000000000000000, -0.000000000000000000 ) ) ;
#20792 = VECTOR ( 'NONE', #5369, 1000.000000000000000 ) ;
#20793 = FACE_OUTER_BOUND ( 'NONE', #7097, .T. ) ;
#20794 = VECTOR ( 'NONE', #7462, 1000.000000000000000 ) ;
#20795 = AXIS2_PLACEMENT_3D ( 'NONE', #12346, #12439, #17428 ) ;
#20796 = FACE_OUTER_BOUND ( 'NONE', #19047, .T. ) ;
#20797 = DIRECTION ( 'NONE',  ( 0.000000000000000000, 0.000000000000000000, -1.000000000000000000 ) ) ;
#20798 = CARTESIAN_POINT ( 'NONE',  ( 0.000000000000000000, 0.000000000000000000, 0.000000000000000000 ) ) ;
#20799 = VERTEX_POINT ( 'NONE', #7037 ) ;
#20800 = EDGE_CURVE ( 'NONE', #3621, #17553, #14087, .T. ) ;
#20801 = EDGE_CURVE ( 'NONE', #3708, #10821, #2056, .T. ) ;
#20802 = EDGE_CURVE ( 'NONE', #11838, #15174, #3161, .T. ) ;
#20803 = DIRECTION ( 'NONE',  ( 0.000000000000000000, 0.000000000000000000, 1.000000000000000000 ) ) ;
#20804 = AXIS2_PLACEMENT_3D ( 'NONE', #6118, #2804, #7661 ) ;
#20805 = ADVANCED_FACE ( 'NONE', ( #20610, #4025 ), #17522, .F. ) ;
#20806 = DIRECTION ( 'NONE',  ( 1.000000000000000000, 0.000000000000000000, 0.000000000000000000 ) ) ;
#20807 = ORIENTED_EDGE ( 'NONE', *, *, #2382, .T. ) ;
#20808 = AXIS2_PLACEMENT_3D ( 'NONE', #13623, #13178, #11539 ) ;
#20809 = DIRECTION ( 'NONE',  ( -1.000000000000000000, 0.000000000000000000, -0.000000000000000000 ) ) ;
#20810 = CIRCLE ( 'NONE', #2462, 44.99999999999999289 ) ;
#20811 = VERTEX_POINT ( 'NONE', #2484 ) ;
#20812 = DIRECTION ( 'NONE',  ( 0.000000000000000000, -0.7880107536067275653, 0.6156614753256510753 ) ) ;
#20813 = ORIENTED_EDGE ( 'NONE', *, *, #14739, .F. ) ;
#20814 = ORIENTED_EDGE ( 'NONE', *, *, #9452, .T. ) ;
#20815 = DIRECTION ( 'NONE',  ( 1.000000000000000000, 0.000000000000000000, 0.000000000000000000 ) ) ;
#20816 = EDGE_CURVE ( 'NONE', #16786, #16161, #21161, .T. ) ;
#20817 = CYLINDRICAL_SURFACE ( 'NONE', #10736, 88.00000000000000000 ) ;
#20818 = CARTESIAN_POINT ( 'NONE',  ( 0.000000000000000000, 0.000000000000000000, 0.000000000000000000 ) ) ;
#20819 = CARTESIAN_POINT ( 'NONE',  ( 10.00000000000000000, -73.32282170386815778, -48.65967342042856103 ) ) ;
#20820 = DIRECTION ( 'NONE',  ( 1.000000000000000000, 0.000000000000000000, 0.000000000000000000 ) ) ;
#20821 = DIRECTION ( 'NONE',  ( -0.000000000000000000, -0.000000000000000000, -1.000000000000000000 ) ) ;
#20822 = EDGE_CURVE ( 'NONE', #8047, #20435, #5804, .T. ) ;
#20823 = CARTESIAN_POINT ( 'NONE',  ( 9.999999999999994671, 0.000000000000000000, 0.000000000000000000 ) ) ;
#20824 = AXIS2_PLACEMENT_3D ( 'NONE', #7533, #16152, #11289 ) ;
#20825 = ORIENTED_EDGE ( 'NONE', *, *, #16804, .T. ) ;
#20826 = CARTESIAN_POINT ( 'NONE',  ( 0.000000000000000000, 8.134922360107273320, -84.67002113262471141 ) ) ;
#20827 = ORIENTED_EDGE ( 'NONE', *, *, #20581, .F. ) ;
#20828 = CARTESIAN_POINT ( 'NONE',  ( 10.00000000000000000, 0.000000000000000000, 0.000000000000000000 ) ) ;
#20829 = ORIENTED_EDGE ( 'NONE', *, *, #4189, .F. ) ;
#20830 = ADVANCED_FACE ( 'NONE', ( #2156 ), #15629, .T. ) ;
#20831 = DIRECTION ( 'NONE',  ( 0.000000000000000000, 0.000000000000000000, -1.000000000000000000 ) ) ;
#20832 = DIRECTION ( 'NONE',  ( 1.000000000000000000, -0.000000000000000000, 0.000000000000000000 ) ) ;
#20833 = MANIFOLD_SOLID_BREP ( 'Cut-Extrude1', #10070 ) ;
#20834 = ORIENTED_EDGE ( 'NONE', *, *, #16216, .F. ) ;
#20835 = VERTEX_POINT ( 'NONE', #9640 ) ;
#20836 = ORIENTED_EDGE ( 'NONE', *, *, #17859, .F. ) ;
#20837 = ORIENTED_EDGE ( 'NONE', *, *, #18011, .F. ) ;
#20838 = FACE_OUTER_BOUND ( 'NONE', #11951, .T. ) ;
#20839 = DIRECTION ( 'NONE',  ( 0.000000000000000000, -0.7880107536067275653, 0.6156614753256510753 ) ) ;
#20840 = VERTEX_POINT ( 'NONE', #9211 ) ;
#20841 = ADVANCED_FACE ( 'NONE', ( #18175 ), #8466, .T. ) ;
#20842 = DIRECTION ( 'NONE',  ( -1.000000000000000000, 0.000000000000000000, 0.000000000000000000 ) ) ;
#20843 = CARTESIAN_POINT ( 'NONE',  ( -1.129531546211690385, 8.434754829127421589E-16, 6.887500000000022382 ) ) ;
#20844 = DIRECTION ( 'NONE',  ( -1.000000000000000000, 0.000000000000000000, 0.000000000000000000 ) ) ;
#20845 = EDGE_CURVE ( 'NONE', #9349, #5274, #19404, .T. ) ;
#20846 = DIRECTION ( 'NONE',  ( 0.000000000000000000, -0.2079116908177664480, 0.9781476007338041345 ) ) ;
#20847 = DIRECTION ( 'NONE',  ( -1.000000000000000000, -0.000000000000000000, 0.000000000000000000 ) ) ;
#20848 = ADVANCED_FACE ( 'NONE', ( #19490 ), #4357, .F. ) ;
#20849 = EDGE_LOOP ( 'NONE', ( #15336, #17626, #3167, #2558 ) ) ;
#20850 = EDGE_CURVE ( 'NONE', #10454, #3353, #9869, .T. ) ;
#20851 = DIRECTION ( 'NONE',  ( -0.000000000000000000, -0.000000000000000000, -1.000000000000000000 ) ) ;
#20852 = CARTESIAN_POINT ( 'NONE',  ( -123.5000000000000142, 1.512438796946981289E-14, -3.000000000000000000 ) ) ;
#20853 = DIRECTION ( 'NONE',  ( -1.000000000000000000, 0.000000000000000000, 0.000000000000000000 ) ) ;
#20854 = VERTEX_POINT ( 'NONE', #17845 ) ;
#20855 = FACE_BOUND ( 'NONE', #14029, .T. ) ;
#20856 = ORIENTED_EDGE ( 'NONE', *, *, #14306, .T. ) ;
#20857 = DIRECTION ( 'NONE',  ( -1.000000000000000000, -0.000000000000000000, 0.000000000000000000 ) ) ;
#20858 = ORIENTED_EDGE ( 'NONE', *, *, #6093, .T. ) ;
#20859 = ORIENTED_EDGE ( 'NONE', *, *, #6648, .F. ) ;
#20860 = ORIENTED_EDGE ( 'NONE', *, *, #10313, .F. ) ;
#20861 = CARTESIAN_POINT ( 'NONE',  ( 1.500000000000001332, 6.775741118407465085E-16, -5.453125000000000000 ) ) ;
#20862 = ORIENTED_EDGE ( 'NONE', *, *, #10388, .F. ) ;
#20863 = CARTESIAN_POINT ( 'NONE',  ( 10.00000000000000000, -25.56104204395249369, -81.12843256239690959 ) ) ;
#20864 = CYLINDRICAL_SURFACE ( 'NONE', #10756, 113.8250000000000028 ) ;
#20865 = DIRECTION ( 'NONE',  ( 0.000000000000000000, 0.9993908270190957621, -0.03489949670249752750 ) ) ;
#20866 = STYLED_ITEM ( 'NONE', ( #13745 ), #6437 ) ;
#20867 = DIRECTION ( 'NONE',  ( 0.000000000000000000, 0.000000000000000000, -1.000000000000000000 ) ) ;
#20868 = CARTESIAN_POINT ( 'NONE',  ( 10.00000000000000000, 78.04699792498145428, 49.64978465107317618 ) ) ;
#20869 = CARTESIAN_POINT ( 'NONE',  ( 5.000000000000000000, 85.54350296776112828, 20.64725405482881726 ) ) ;
#20870 = DIRECTION ( 'NONE',  ( 0.000000000000000000, -1.000000000000000000, 0.000000000000000000 ) ) ;
#20871 = CARTESIAN_POINT ( 'NONE',  ( 10.00000000000000000, -26.69209308833512395, 6.612652082459228531 ) ) ;
#20872 = CARTESIAN_POINT ( 'NONE',  ( 7.500000000000000000, 9.184850993605147944E-16, 0.000000000000000000 ) ) ;
#20873 = EDGE_LOOP ( 'NONE', ( #15720, #5351, #7357, #20664 ) ) ;
#20874 = CARTESIAN_POINT ( 'NONE',  ( 10.00000000000000000, -57.53593069156319473, -72.42963261301021305 ) ) ;
#20875 = ORIENTED_EDGE ( 'NONE', *, *, #12559, .T. ) ;
#20876 = CIRCLE ( 'NONE', #11350, 113.8250000000000028 ) ;
#20877 = VERTEX_POINT ( 'NONE', #4681 ) ;
#20878 = ORIENTED_EDGE ( 'NONE', *, *, #395, .F. ) ;
#20879 = ORIENTED_EDGE ( 'NONE', *, *, #15564, .T. ) ;
#20880 = VERTEX_POINT ( 'NONE', #2699 ) ;
#20881 = ORIENTED_EDGE ( 'NONE', *, *, #864, .T. ) ;
#20882 = AXIS2_PLACEMENT_3D ( 'NONE', #13224, #15210, #19975 ) ;
#20883 = CIRCLE ( 'NONE', #11358, 115.1000000000000227 ) ;
#20884 = LINE ( 'NONE', #1000, #20050 ) ;
#20885 = EDGE_LOOP ( 'NONE', ( #21771, #21166, #12746, #18150 ) ) ;
#20886 = CYLINDRICAL_SURFACE ( 'NONE', #7622, 88.00000000000000000 ) ;
#20887 = DIRECTION ( 'NONE',  ( 0.000000000000000000, 0.000000000000000000, 1.000000000000000000 ) ) ;
#20888 = CARTESIAN_POINT ( 'NONE',  ( 0.000000000000000000, -81.83745710415254848, -32.35167097270233683 ) ) ;
#20889 = CARTESIAN_POINT ( 'NONE',  ( 0.000000000000000000, 0.000000000000000000, 3.000000000000000000 ) ) ;
#20890 = EDGE_CURVE ( 'NONE', #9457, #14635, #358, .T. ) ;
#20891 = DIRECTION ( 'NONE',  ( -1.000000000000000000, -0.000000000000000000, -0.000000000000000000 ) ) ;
#20892 = CYLINDRICAL_SURFACE ( 'NONE', #16444, 92.50100000000000477 ) ;
#20893 = CARTESIAN_POINT ( 'NONE',  ( 0.000000000000000000, 60.00000000000000000, -15.00000000000000000 ) ) ;
#20894 = CARTESIAN_POINT ( 'NONE',  ( 10.00000000000000000, 10.41137886060107576, 91.91321010181850681 ) ) ;
#20895 = CIRCLE ( 'NONE', #4668, 44.99999999999999289 ) ;
#20896 = ORIENTED_EDGE ( 'NONE', *, *, #14819, .T. ) ;
#20897 = MANIFOLD_SOLID_BREP ( 'InnerRace', #20326 ) ;
#20898 = EDGE_CURVE ( 'NONE', #4038, #8443, #18287, .T. ) ;
#20899 = DIRECTION ( 'NONE',  ( 1.000000000000000000, 0.000000000000000000, 0.000000000000000000 ) ) ;
#20900 = CIRCLE ( 'NONE', #18782, 88.00000000000000000 ) ;
#20901 = CIRCLE ( 'NONE', #7846, 44.99999999999998579 ) ;
#20902 = FACE_OUTER_BOUND ( 'NONE', #7900, .T. ) ;
#20903 = CARTESIAN_POINT ( 'NONE',  ( 5.000000000000000888, -28.00896854772002342, 15.47571261340914539 ) ) ;
#20904 = ORIENTED_EDGE ( 'NONE', *, *, #440, .F. ) ;
#20905 = DIRECTION ( 'NONE',  ( 0.000000000000000000, -1.000000000000000000, 0.000000000000000000 ) ) ;
#20906 = ORIENTED_EDGE ( 'NONE', *, *, #10825, .F. ) ;
#20907 = DIRECTION ( 'NONE',  ( 0.000000000000000000, 0.000000000000000000, -1.000000000000000000 ) ) ;
#20908 = AXIS2_PLACEMENT_3D ( 'NONE', #20118, #9826, #16911 ) ;
#20909 = ORIENTED_EDGE ( 'NONE', *, *, #13752, .T. ) ;
#20910 = ORIENTED_EDGE ( 'NONE', *, *, #8646, .F. ) ;
#20911 = CARTESIAN_POINT ( 'NONE',  ( -1.500000000000001332, 6.775741118407465085E-16, 5.453125000000000000 ) ) ;
#20912 = CARTESIAN_POINT ( 'NONE',  ( 10.00000000000000000, 0.000000000000000000, 0.000000000000000000 ) ) ;
#20913 = AXIS2_PLACEMENT_3D ( 'NONE', #7082, #3863, #13809 ) ;
#20914 = AXIS2_PLACEMENT_3D ( 'NONE', #6533, #15340, #13361 ) ;
#20915 = LINE ( 'NONE', #3801, #14265 ) ;
#20916 = CARTESIAN_POINT ( 'NONE',  ( -90.00000000000000000, 0.000000000000000000, -120.0000000000000426 ) ) ;
#20917 = EDGE_CURVE ( 'NONE', #5377, #15908, #12858, .T. ) ;
#20918 = EDGE_CURVE ( 'NONE', #14957, #4858, #3178, .T. ) ;
#20919 = CYLINDRICAL_SURFACE ( 'NONE', #8664, 44.99999999999999289 ) ;
#20920 = DIRECTION ( 'NONE',  ( 0.000000000000000000, -0.5877852522924632561, -0.8090169943749545567 ) ) ;
#20921 = AXIS2_PLACEMENT_3D ( 'NONE', #3794, #14066, #7116 ) ;
#20922 = CARTESIAN_POINT ( 'NONE',  ( 0.000000000000000000, -1.592605004252988898, 28.14575649959894221 ) ) ;
#20923 = DIRECTION ( 'NONE',  ( 1.000000000000000000, 0.000000000000000000, 0.000000000000000000 ) ) ;
#20924 = CARTESIAN_POINT ( 'NONE',  ( 1.399999999999998579, 0.000000000000000000, 0.000000000000000000 ) ) ;
#20925 = AXIS2_PLACEMENT_3D ( 'NONE', #12382, #17588, #9067 ) ;
#20926 = ORIENTED_EDGE ( 'NONE', *, *, #16700, .T. ) ;
#20927 = DIRECTION ( 'NONE',  ( 0.000000000000000000, 0.000000000000000000, 1.000000000000000000 ) ) ;
#20928 = COLOUR_RGB ( '', 0.31764706, 0.68627451, 0.89019608) ;
#20929 = ORIENTED_EDGE ( 'NONE', *, *, #21523, .T. ) ;
#20930 = DIRECTION ( 'NONE',  ( 0.000000000000000000, 0.000000000000000000, -1.000000000000000000 ) ) ;
#20931 = ADVANCED_FACE ( 'NONE', ( #19929 ), #16615, .F. ) ;
#20932 = VERTEX_POINT ( 'NONE', #6790 ) ;
#20933 = AXIS2_PLACEMENT_3D ( 'NONE', #16879, #11795, #8161 ) ;
#20934 = DIRECTION ( 'NONE',  ( 0.000000000000000000, 0.000000000000000000, 1.000000000000000000 ) ) ;
#20935 = DIRECTION ( 'NONE',  ( -1.000000000000000000, 0.000000000000000000, 0.000000000000000000 ) ) ;
#20936 = VERTEX_POINT ( 'NONE', #4798 ) ;
#20937 = CIRCLE ( 'NONE', #21646, 11.99999999999999822 ) ;
#20938 = EDGE_CURVE ( 'NONE', #9562, #1096, #3239, .T. ) ;
#20939 = CIRCLE ( 'NONE', #13173, 44.99999999999999289 ) ;
#20940 = EDGE_LOOP ( 'NONE', ( #2886, #10665, #11813, #8713 ) ) ;
#20941 = ORIENTED_EDGE ( 'NONE', *, *, #6624, .T. ) ;
#20942 = ORIENTED_EDGE ( 'NONE', *, *, #15668, .T. ) ;
#20943 = CARTESIAN_POINT ( 'NONE',  ( 10.00000000000000000, -27.82509854686814066, 4.525913221811051379 ) ) ;
#20944 = CARTESIAN_POINT ( 'NONE',  ( 10.00000000000000000, -27.40684453873954851, -16.51862198942037097 ) ) ;
#20945 = ORIENTED_EDGE ( 'NONE', *, *, #7306, .T. ) ;
#20946 = CIRCLE ( 'NONE', #494, 88.00000000000000000 ) ;
#20947 = EDGE_CURVE ( 'NONE', #8227, #10261, #20154, .T. ) ;
#20948 = LINE ( 'NONE', #2384, #15315 ) ;
#20949 = DIRECTION ( 'NONE',  ( 1.000000000000000000, 0.000000000000000000, 0.000000000000000000 ) ) ;
#20950 = CARTESIAN_POINT ( 'NONE',  ( 1.500000000000000000, 5.000000000000004441, 4.769696007084728073 ) ) ;
#20951 = EDGE_CURVE ( 'NONE', #1558, #374, #11747, .T. ) ;
#20952 = DIRECTION ( 'NONE',  ( 1.000000000000000000, 0.000000000000000000, 0.000000000000000000 ) ) ;
#20953 = DIRECTION ( 'NONE',  ( -1.000000000000000000, -0.000000000000000000, -0.000000000000000000 ) ) ;
#20954 = ADVANCED_FACE ( 'NONE', ( #11971 ), #1473, .T. ) ;
#20955 = ORIENTED_EDGE ( 'NONE', *, *, #18891, .T. ) ;
#20956 = FACE_OUTER_BOUND ( 'NONE', #19520, .T. ) ;
#20957 = DIRECTION ( 'NONE',  ( 0.000000000000000000, 0.000000000000000000, 1.000000000000000000 ) ) ;
#20958 = DIRECTION ( 'NONE',  ( 0.000000000000000000, 0.000000000000000000, 1.000000000000000000 ) ) ;
#20959 = EDGE_CURVE ( 'NONE', #827, #19897, #9513, .T. ) ;
#20960 = ORIENTED_EDGE ( 'NONE', *, *, #552, .F. ) ;
#20961 = AXIS2_PLACEMENT_3D ( 'NONE', #13854, #20712, #5575 ) ;
#20962 = CARTESIAN_POINT ( 'NONE',  ( 5.000000000000000000, -19.29292659244022445, 25.53004080487755800 ) ) ;
#20963 = EDGE_LOOP ( 'NONE', ( #1117, #10656 ) ) ;
#20964 = LINE ( 'NONE', #19519, #3125 ) ;
#20965 = EDGE_CURVE ( 'NONE', #19585, #8691, #20045, .T. ) ;
#20966 = ORIENTED_EDGE ( 'NONE', *, *, #5024, .F. ) ;
#20967 = VECTOR ( 'NONE', #10570, 1000.000000000000000 ) ;
#20968 = ORIENTED_EDGE ( 'NONE', *, *, #4465, .T. ) ;
#20969 = ORIENTED_EDGE ( 'NONE', *, *, #16182, .F. ) ;
#20970 = FACE_OUTER_BOUND ( 'NONE', #17399, .T. ) ;
#20971 = AXIS2_PLACEMENT_3D ( 'NONE', #7543, #5567, #9091 ) ;
#20972 = EDGE_CURVE ( 'NONE', #5686, #11788, #1063, .T. ) ;
#20973 = ORIENTED_EDGE ( 'NONE', *, *, #5270, .F. ) ;
#20974 = DIRECTION ( 'NONE',  ( 0.000000000000000000, 1.000000000000000000, -1.224646799147353207E-16 ) ) ;
#20975 = CARTESIAN_POINT ( 'NONE',  ( 10.00000000000000000, 92.32475887865433606, -5.707354816229567973 ) ) ;
#20976 = DIRECTION ( 'NONE',  ( 1.000000000000000000, 0.000000000000000000, 0.000000000000000000 ) ) ;
#20977 = CARTESIAN_POINT ( 'NONE',  ( 10.00000000000000000, -83.03980459022491800, 18.42770452393216374 ) ) ;
#20978 = AXIS2_PLACEMENT_3D ( 'NONE', #21361, #6356, #17947 ) ;
#20979 = FACE_OUTER_BOUND ( 'NONE', #2724, .T. ) ;
#20980 = EDGE_CURVE ( 'NONE', #4497, #6588, #3882, .T. ) ;
#20981 = DIRECTION ( 'NONE',  ( 0.000000000000000000, 0.7880107536067190166, 0.6156614753256620665 ) ) ;
#20982 = VECTOR ( 'NONE', #5761, 1000.000000000000000 ) ;
#20983 = LINE ( 'NONE', #4522, #876 ) ;
#20984 = AXIS2_PLACEMENT_3D ( 'NONE', #7324, #8752, #3568 ) ;
#20985 = CARTESIAN_POINT ( 'NONE',  ( 10.00000000000000000, 85.54350296776112828, 20.64725405482881726 ) ) ;
#20986 = CARTESIAN_POINT ( 'NONE',  ( -10.00000000000000000, 0.000000000000000000, 0.000000000000000000 ) ) ;
#20987 = AXIS2_PLACEMENT_3D ( 'NONE', #7229, #7343, #17391 ) ;
#20988 = VECTOR ( 'NONE', #20091, 1000.000000000000000 ) ;
#20989 = DIRECTION ( 'NONE',  ( -1.000000000000000000, -0.000000000000000000, -0.000000000000000000 ) ) ;
#20990 = ORIENTED_EDGE ( 'NONE', *, *, #17606, .F. ) ;
#20991 = VERTEX_POINT ( 'NONE', #11650 ) ;
#20992 = ORIENTED_EDGE ( 'NONE', *, *, #7981, .F. ) ;
#20993 = CIRCLE ( 'NONE', #6890, 45.00000000000000000 ) ;
#20994 = VERTEX_POINT ( 'NONE', #8120 ) ;
#20995 = AXIS2_PLACEMENT_3D ( 'NONE', #5182, #3846, #7063 ) ;
#20996 = CIRCLE ( 'NONE', #1256, 44.99999999999999289 ) ;
#20997 = EDGE_CURVE ( 'NONE', #14473, #8443, #17300, .T. ) ;
#20998 = VERTEX_POINT ( 'NONE', #20262 ) ;
#20999 = CIRCLE ( 'NONE', #14657, 44.99999999999998579 ) ;
#21000 = CARTESIAN_POINT ( 'NONE',  ( 0.000000000000000000, 60.65655256511237781, 59.63197188857542841 ) ) ;
#21001 = ORIENTED_EDGE ( 'NONE', *, *, #9706, .F. ) ;
#21002 = DIRECTION ( 'NONE',  ( 1.000000000000000000, 0.000000000000000000, 0.000000000000000000 ) ) ;
#21003 = AXIS2_PLACEMENT_3D ( 'NONE', #21414, #4624, #11581 ) ;
#21004 = FACE_OUTER_BOUND ( 'NONE', #10932, .T. ) ;
#21005 = DIRECTION ( 'NONE',  ( 1.000000000000000000, -0.000000000000000000, -0.000000000000000000 ) ) ;
#21006 = DIRECTION ( 'NONE',  ( 0.000000000000000000, 0.000000000000000000, 1.000000000000000000 ) ) ;
#21007 = CARTESIAN_POINT ( 'NONE',  ( 0.000000000000000000, 92.22057093985038989, -7.197311757039553726 ) ) ;
#21008 = CIRCLE ( 'NONE', #3373, 45.00000000000000000 ) ;
#21009 = FACE_OUTER_BOUND ( 'NONE', #21810, .T. ) ;
#21010 = DIRECTION ( 'NONE',  ( -1.000000000000000000, -0.000000000000000000, -0.000000000000000000 ) ) ;
#21011 = CARTESIAN_POINT ( 'NONE',  ( 10.00000000000000000, 22.77465461094694632, -15.41136296218063428 ) ) ;
#21012 = VERTEX_POINT ( 'NONE', #15061 ) ;
#21013 = VECTOR ( 'NONE', #18497, 1000.000000000000000 ) ;
#21014 = AXIS2_PLACEMENT_3D ( 'NONE', #6022, #4342, #17720 ) ;
#21015 = DIRECTION ( 'NONE',  ( 0.000000000000000000, -0.5299192642332118952, 0.8480480961564216269 ) ) ;
#21016 = CIRCLE ( 'NONE', #14303, 88.00000000000000000 ) ;
#21017 = DIRECTION ( 'NONE',  ( 1.000000000000000000, 0.000000000000000000, -0.000000000000000000 ) ) ;
#21018 = LINE ( 'NONE', #12498, #3541 ) ;
#21019 = ORIENTED_EDGE ( 'NONE', *, *, #18765, .F. ) ;
#21020 = DIRECTION ( 'NONE',  ( -0.000000000000000000, -1.000000000000000000, -0.000000000000000000 ) ) ;
#21021 = ORIENTED_EDGE ( 'NONE', *, *, #17937, .F. ) ;
#21022 = CARTESIAN_POINT ( 'NONE',  ( 1.932673851087414390E-15, 28.49999999999999645, -1.129446232850617009E-14 ) ) ;
#21023 = DIRECTION ( 'NONE',  ( 0.000000000000000000, 0.06975647374412546897, -0.9975640502598241977 ) ) ;
#21024 = EDGE_LOOP ( 'NONE', ( #18825, #15581, #20541, #7354 ) ) ;
#21025 = CIRCLE ( 'NONE', #13611, 32.00000000000000000 ) ;
#21026 = ORIENTED_EDGE ( 'NONE', *, *, #6069, .T. ) ;
#21027 = CARTESIAN_POINT ( 'NONE',  ( 10.00000000000000000, 0.000000000000000000, 0.000000000000000000 ) ) ;
#21028 = VECTOR ( 'NONE', #6030, 1000.000000000000000 ) ;
#21029 = EDGE_CURVE ( 'NONE', #9001, #17402, #18495, .T. ) ;
#21030 = DIRECTION ( 'NONE',  ( -1.000000000000000000, -0.000000000000000000, -0.000000000000000000 ) ) ;
#21031 = AXIS2_PLACEMENT_3D ( 'NONE', #7285, #12677, #14012 ) ;
#21032 = DIRECTION ( 'NONE',  ( 0.000000000000000000, 0.000000000000000000, 1.000000000000000000 ) ) ;
#21033 = CARTESIAN_POINT ( 'NONE',  ( 10.00000000000000000, 0.000000000000000000, 0.000000000000000000 ) ) ;
#21034 = DIRECTION ( 'NONE',  ( -1.000000000000000000, -0.000000000000000000, 0.000000000000000000 ) ) ;
#21035 = DIRECTION ( 'NONE',  ( 0.000000000000000000, 0.000000000000000000, 1.000000000000000000 ) ) ;
#21036 = FACE_OUTER_BOUND ( 'NONE', #11757, .T. ) ;
#21037 = DIRECTION ( 'NONE',  ( -1.000000000000000000, -0.000000000000000000, 0.000000000000000000 ) ) ;
#21038 = CARTESIAN_POINT ( 'NONE',  ( 2.799999999999996714, 60.00000000000000000, -15.00000000000000000 ) ) ;
#21039 = ORIENTED_EDGE ( 'NONE', *, *, #4279, .F. ) ;
#21040 = DIRECTION ( 'NONE',  ( -1.000000000000000000, 0.000000000000000000, 0.000000000000000000 ) ) ;
#21041 = ORIENTED_EDGE ( 'NONE', *, *, #20234, .F. ) ;
#21042 = CIRCLE ( 'NONE', #13277, 44.99999999999998579 ) ;
#21043 = VECTOR ( 'NONE', #1549, 1000.000000000000000 ) ;
#21044 = VECTOR ( 'NONE', #12115, 1000.000000000000000 ) ;
#21045 = DIRECTION ( 'NONE',  ( -1.000000000000000000, -0.000000000000000000, -0.000000000000000000 ) ) ;
#21046 = ORIENTED_EDGE ( 'NONE', *, *, #5738, .F. ) ;
#21047 = ADVANCED_FACE ( 'NONE', ( #1806 ), #10084, .F. ) ;
#21048 = DIRECTION ( 'NONE',  ( -1.000000000000000000, 0.000000000000000000, 0.000000000000000000 ) ) ;
#21049 = ORIENTED_EDGE ( 'NONE', *, *, #2874, .T. ) ;
#21050 = VERTEX_POINT ( 'NONE', #6462 ) ;
#21051 = ORIENTED_EDGE ( 'NONE', *, *, #15248, .T. ) ;
#21052 = VERTEX_POINT ( 'NONE', #3465 ) ;
#21053 = DIRECTION ( 'NONE',  ( 0.000000000000000000, 0.000000000000000000, -1.000000000000000000 ) ) ;
#21054 = CARTESIAN_POINT ( 'NONE',  ( 5.000000000000002665, -23.62010150527279961, 84.77081340225898032 ) ) ;
#21055 = EDGE_CURVE ( 'NONE', #10855, #21383, #2460, .T. ) ;
#21056 = ORIENTED_EDGE ( 'NONE', *, *, #14465, .F. ) ;
#21057 = CIRCLE ( 'NONE', #12937, 88.00000000000000000 ) ;
#21058 = DIRECTION ( 'NONE',  ( -1.000000000000000000, 0.000000000000000000, -0.000000000000000000 ) ) ;
#21059 = DIRECTION ( 'NONE',  ( 0.000000000000000000, 0.6946583704589934793, 0.7193398003386547446 ) ) ;
#21060 = CIRCLE ( 'NONE', #6599, 44.99999999999999289 ) ;
#21061 = DIRECTION ( 'NONE',  ( 0.000000000000000000, 1.603655480014115143E-14, -1.000000000000000000 ) ) ;
#21062 = CARTESIAN_POINT ( 'NONE',  ( 1.500000000000001332, 9.123618653647806797E-16, 7.400000000000020783 ) ) ;
#21063 = VECTOR ( 'NONE', #3752, 1000.000000000000000 ) ;
#21064 = CARTESIAN_POINT ( 'NONE',  ( 0.000000000000000000, 30.71797041605924505, -82.46457599186518905 ) ) ;
#21065 = EDGE_CURVE ( 'NONE', #21597, #7542, #7407, .T. ) ;
#21066 = ORIENTED_EDGE ( 'NONE', *, *, #6776, .F. ) ;
#21067 = CARTESIAN_POINT ( 'NONE',  ( 10.00000000000000000, 76.53853822674039975, -43.42639941457040464 ) ) ;
#21068 = FACE_OUTER_BOUND ( 'NONE', #3438, .T. ) ;
#21069 = CARTESIAN_POINT ( 'NONE',  ( 10.00000000000000000, 43.18649929580192293, 73.28107340219430910 ) ) ;
#21070 = ORIENTED_EDGE ( 'NONE', *, *, #19566, .F. ) ;
#21071 = AXIS2_PLACEMENT_3D ( 'NONE', #8933, #10702, #11027 ) ;
#21072 = EDGE_CURVE ( 'NONE', #19400, #11293, #5301, .T. ) ;
#21073 = CARTESIAN_POINT ( 'NONE',  ( -1.114300000000000068, 6.898680348956876061E-16, 5.633200000000004870 ) ) ;
#21074 = ADVANCED_FACE ( 'NONE', ( #5775 ), #13839, .T. ) ;
#21075 = AXIS2_PLACEMENT_3D ( 'NONE', #19745, #19841, #21517 ) ;
#21076 = EDGE_CURVE ( 'NONE', #10985, #8423, #18819, .T. ) ;
#21077 = EDGE_LOOP ( 'NONE', ( #7975, #4253, #20878, #19755 ) ) ;
#21078 = CARTESIAN_POINT ( 'NONE',  ( 0.000000000000000000, 0.000000000000000000, 0.000000000000000000 ) ) ;
#21079 = AXIS2_PLACEMENT_3D ( 'NONE', #6515, #16328, #1196 ) ;
#21080 = ORIENTED_EDGE ( 'NONE', *, *, #6253, .F. ) ;
#21081 = EDGE_CURVE ( 'NONE', #3591, #3827, #21175, .T. ) ;
#21082 = ORIENTED_EDGE ( 'NONE', *, *, #8529, .F. ) ;
#21083 = ORIENTED_EDGE ( 'NONE', *, *, #17441, .F. ) ;
#21084 = FACE_OUTER_BOUND ( 'NONE', #11134, .T. ) ;
#21085 = ORIENTED_EDGE ( 'NONE', *, *, #16640, .T. ) ;
#21086 = DIRECTION ( 'NONE',  ( -1.000000000000000000, -0.000000000000000000, -0.000000000000000000 ) ) ;
#21087 = DIRECTION ( 'NONE',  ( -1.000000000000000000, -0.000000000000000000, -0.000000000000000000 ) ) ;
#21088 = CARTESIAN_POINT ( 'NONE',  ( 1.199999999999992628, 8.239576745513314221E-16, 6.728125000000023448 ) ) ;
#21089 = LINE ( 'NONE', #9149, #8936 ) ;
#21090 = EDGE_CURVE ( 'NONE', #4970, #18142, #20122, .T. ) ;
#21091 = CIRCLE ( 'NONE', #2035, 32.00000000000000000 ) ;
#21092 = CYLINDRICAL_SURFACE ( 'NONE', #14227, 11.99999999999999822 ) ;
#21093 = AXIS2_PLACEMENT_3D ( 'NONE', #8991, #2697, #720 ) ;
#21094 = DIRECTION ( 'NONE',  ( -1.000000000000000000, -0.000000000000000000, -0.000000000000000000 ) ) ;
#21095 = DIRECTION ( 'NONE',  ( 1.000000000000000000, 0.000000000000000000, 0.000000000000000000 ) ) ;
#21096 = TOROIDAL_SURFACE ( 'NONE', #21783, 7.400000000000019895, 0.1000000000000006994 ) ;
#21097 = CARTESIAN_POINT ( 'NONE',  ( 10.00000000000000000, -71.72924546249979016, 45.71766382684644725 ) ) ;
#21098 = ADVANCED_FACE ( 'NONE', ( #7006 ), #2345, .F. ) ;
#21099 = CARTESIAN_POINT ( 'NONE',  ( 10.00000000000000000, 19.83954325428658194, 82.71385593638699163 ) ) ;
#21100 = ADVANCED_FACE ( 'NONE', ( #5344 ), #3573, .F. ) ;
#21101 = DIRECTION ( 'NONE',  ( 0.000000000000000000, 0.000000000000000000, 1.000000000000000000 ) ) ;
#21102 = ORIENTED_EDGE ( 'NONE', *, *, #21665, .T. ) ;
#21103 = EDGE_LOOP ( 'NONE', ( #3090, #10998 ) ) ;
#21104 = ORIENTED_EDGE ( 'NONE', *, *, #1864, .F. ) ;
#21105 = VECTOR ( 'NONE', #16697, 1000.000000000000000 ) ;
#21106 = VECTOR ( 'NONE', #4341, 1000.000000000000000 ) ;
#21107 = EDGE_CURVE ( 'NONE', #8068, #1586, #2815, .T. ) ;
#21108 = ORIENTED_EDGE ( 'NONE', *, *, #16726, .F. ) ;
#21109 = CIRCLE ( 'NONE', #11586, 92.50099999999999056 ) ;
#21110 = ORIENTED_EDGE ( 'NONE', *, *, #3290, .T. ) ;
#21111 = CARTESIAN_POINT ( 'NONE',  ( 10.00000000000000000, 2.208823992045340301, -85.03123271466934341 ) ) ;
#21112 = ORIENTED_EDGE ( 'NONE', *, *, #5428, .T. ) ;
#21113 = DIRECTION ( 'NONE',  ( -1.000000000000000000, 0.000000000000000000, 0.000000000000000000 ) ) ;
#21114 = CARTESIAN_POINT ( 'NONE',  ( 10.00000000000000000, 0.000000000000000000, 0.000000000000000000 ) ) ;
#21115 = DIRECTION ( 'NONE',  ( 0.000000000000000000, 0.000000000000000000, 1.000000000000000000 ) ) ;
#21116 = EDGE_CURVE ( 'NONE', #16361, #10612, #5640, .T. ) ;
#21117 = CARTESIAN_POINT ( 'NONE',  ( 0.000000000000000000, 35.34277389771654043, -85.48288328206348297 ) ) ;
#21118 = CARTESIAN_POINT ( 'NONE',  ( 2.000000000000000000, 70.00000000000000000, 9.999999999999998224 ) ) ;
#21119 = DIRECTION ( 'NONE',  ( 0.000000000000000000, 0.000000000000000000, -1.000000000000000000 ) ) ;
#21120 = EDGE_CURVE ( 'NONE', #4745, #12130, #6363, .T. ) ;
#21121 = CARTESIAN_POINT ( 'NONE',  ( 5.000000000000002665, 17.64925110578583300, -86.21197095186326464 ) ) ;
#21122 = FACE_OUTER_BOUND ( 'NONE', #15125, .T. ) ;
#21123 = CARTESIAN_POINT ( 'NONE',  ( 10.00000000000000000, 12.90282758292980247, 25.06465718894781247 ) ) ;
#21124 = VECTOR ( 'NONE', #15127, 1000.000000000000000 ) ;
#21125 = CIRCLE ( 'NONE', #10529, 32.00000000000000000 ) ;
#21127 = EDGE_CURVE ( 'NONE', #21050, #15057, #10411, .T. ) ;
#21126 = AXIS2_PLACEMENT_3D ( 'NONE', #7848, #7962, #14587 ) ;
#21128 = AXIS2_PLACEMENT_3D ( 'NONE', #4887, #9514, #11628 ) ;
#21129 = AXIS2_PLACEMENT_3D ( 'NONE', #7351, #15738, #16968 ) ;
#21130 = ORIENTED_EDGE ( 'NONE', *, *, #937, .F. ) ;
#21131 = VECTOR ( 'NONE', #12714, 1000.000000000000000 ) ;
#21132 = EDGE_CURVE ( 'NONE', #1388, #2507, #6028, .T. ) ;
#21133 = DIRECTION ( 'NONE',  ( 0.000000000000000000, 0.000000000000000000, 1.000000000000000000 ) ) ;
#21134 = CARTESIAN_POINT ( 'NONE',  ( 5.000000000000002665, 76.53853822674039975, -43.42639941457040464 ) ) ;
#21135 = LINE ( 'NONE', #2458, #7085 ) ;
#21136 = ORIENTED_EDGE ( 'NONE', *, *, #5142, .T. ) ;
#21137 = AXIS2_PLACEMENT_3D ( 'NONE', #17865, #17650, #12877 ) ;
#21138 = DIRECTION ( 'NONE',  ( 0.000000000000000000, -0.4694715627858797591, -0.8829475928589327616 ) ) ;
#21139 = ORIENTED_EDGE ( 'NONE', *, *, #6495, .T. ) ;
#21140 = EDGE_LOOP ( 'NONE', ( #21428, #13932, #6582, #3698 ) ) ;
#21141 = CARTESIAN_POINT ( 'NONE',  ( -4.747323942153193429E-17, 30.00000000000000000, -8.986485741053880097E-15 ) ) ;
#21142 = CIRCLE ( 'NONE', #2780, 32.00000000000000000 ) ;
#21143 = CARTESIAN_POINT ( 'NONE',  ( 5.000000000000002665, 83.89484365856945658, -26.56417150042864961 ) ) ;
#21144 = ORIENTED_EDGE ( 'NONE', *, *, #4737, .T. ) ;
#21145 = ORIENTED_EDGE ( 'NONE', *, *, #9012, .F. ) ;
#21146 = CYLINDRICAL_SURFACE ( 'NONE', #15320, 32.00000000000000000 ) ;
#21147 = AXIS2_PLACEMENT_3D ( 'NONE', #12445, #14215, #18878 ) ;
#21148 = CIRCLE ( 'NONE', #5265, 44.99999999999999289 ) ;
#21149 = CARTESIAN_POINT ( 'NONE',  ( -1.399999999999999911, 0.000000000000000000, -5.100000000000000533 ) ) ;
#21150 = DIRECTION ( 'NONE',  ( 1.000000000000000000, 0.000000000000000000, -0.000000000000000000 ) ) ;
#21151 = CARTESIAN_POINT ( 'NONE',  ( -10.00000000000002309, 0.000000000000000000, -113.8250000000000028 ) ) ;
#21152 = DIRECTION ( 'NONE',  ( 1.000000000000000000, 0.000000000000000000, 0.000000000000000000 ) ) ;
#21153 = CARTESIAN_POINT ( 'NONE',  ( 0.000000000000000000, 85.22372865846323009, -21.92979875759543162 ) ) ;
#21154 = CARTESIAN_POINT ( 'NONE',  ( 0.000000000000000000, 0.000000000000000000, 0.000000000000000000 ) ) ;
#21155 = CARTESIAN_POINT ( 'NONE',  ( 10.00000000000000000, 0.000000000000000000, 0.000000000000000000 ) ) ;
#21156 = LINE ( 'NONE', #15948, #20393 ) ;
#21157 = ORIENTED_EDGE ( 'NONE', *, *, #3392, .T. ) ;
#21158 = CARTESIAN_POINT ( 'NONE',  ( 10.00000000000000000, 56.35896156214949571, 73.34918167666329225 ) ) ;
#21159 = CIRCLE ( 'NONE', #5990, 11.99999999999999822 ) ;
#21160 = ORIENTED_EDGE ( 'NONE', *, *, #9350, .F. ) ;
#21161 = CIRCLE ( 'NONE', #18349, 88.00000000000000000 ) ;
#21162 = DIRECTION ( 'NONE',  ( -1.000000000000000000, 0.000000000000000000, 0.000000000000000000 ) ) ;
#21163 = PRESENTATION_STYLE_ASSIGNMENT (( #14410 ) ) ;
#21164 = CARTESIAN_POINT ( 'NONE',  ( 10.00000000000000000, -57.06999622551760609, -66.98518889142141575 ) ) ;
#21165 = ORIENTED_EDGE ( 'NONE', *, *, #8007, .T. ) ;
#21166 = ORIENTED_EDGE ( 'NONE', *, *, #21373, .F. ) ;
#21167 = ORIENTED_EDGE ( 'NONE', *, *, #4317, .T. ) ;
#21168 = VERTEX_POINT ( 'NONE', #7112 ) ;
#21169 = CARTESIAN_POINT ( 'NONE',  ( 0.000000000000000000, 27.82509854686811224, 4.525913221811229903 ) ) ;
#21170 = DIRECTION ( 'NONE',  ( -1.000000000000000000, 0.000000000000000000, 0.000000000000000000 ) ) ;
#21171 = ORIENTED_EDGE ( 'NONE', *, *, #2094, .T. ) ;
#21172 = CARTESIAN_POINT ( 'NONE',  ( 10.00000000000000888, 2.828427124746190291, 1.000000000000000000 ) ) ;
#21173 = CARTESIAN_POINT ( 'NONE',  ( 0.000000000000000000, -73.32282170386815778, -48.65967342042856103 ) ) ;
#21174 = DIRECTION ( 'NONE',  ( 0.000000000000000000, 0.4067366430757946572, 0.9135454576426033091 ) ) ;
#21175 = CIRCLE ( 'NONE', #4581, 11.99999999999999822 ) ;
#21176 = CARTESIAN_POINT ( 'NONE',  ( 10.00000000000000000, -9.366510754379051562, -25.85466064925435603 ) ) ;
#21177 = CARTESIAN_POINT ( 'NONE',  ( 10.00000000000000000, 17.64925110578469258, 86.21197095186350623 ) ) ;
#21178 = EDGE_CURVE ( 'NONE', #428, #11955, #20583, .T. ) ;
#21179 = ORIENTED_EDGE ( 'NONE', *, *, #19216, .T. ) ;
#21180 = DIRECTION ( 'NONE',  ( -1.000000000000000000, -0.000000000000000000, -0.000000000000000000 ) ) ;
#21181 = CARTESIAN_POINT ( 'NONE',  ( 10.00000000000000000, 0.000000000000000000, 0.000000000000000000 ) ) ;
#21182 = EDGE_CURVE ( 'NONE', #16217, #1841, #10239, .T. ) ;
#21183 = FACE_OUTER_BOUND ( 'NONE', #10931, .T. ) ;
#21184 = ORIENTED_EDGE ( 'NONE', *, *, #6106, .T. ) ;
#21185 = CARTESIAN_POINT ( 'NONE',  ( 10.00000000000000000, -11.59241532900569993, -87.23311244498751194 ) ) ;
#21186 = ORIENTED_EDGE ( 'NONE', *, *, #1496, .T. ) ;
#21187 = AXIS2_PLACEMENT_3D ( 'NONE', #6666, #5098, #13382 ) ;
#21188 = DIRECTION ( 'NONE',  ( 0.000000000000000000, 0.000000000000000000, 1.000000000000000000 ) ) ;
#21189 = VERTEX_POINT ( 'NONE', #12391 ) ;
#21190 = DIRECTION ( 'NONE',  ( 0.000000000000000000, 0.4067366430757946572, 0.9135454576426033091 ) ) ;
#21191 = ORIENTED_EDGE ( 'NONE', *, *, #9993, .F. ) ;
#21192 = VERTEX_POINT ( 'NONE', #20695 ) ;
#21193 = DIRECTION ( 'NONE',  ( 1.000000000000000000, 0.000000000000000000, 0.000000000000000000 ) ) ;
#21194 = ORIENTED_EDGE ( 'NONE', *, *, #4288, .F. ) ;
#21195 = CARTESIAN_POINT ( 'NONE',  ( 0.000000000000000000, 28.15804365424197186, 10.64184787299392454 ) ) ;
#21196 = DIRECTION ( 'NONE',  ( 1.000000000000000000, 0.000000000000000000, 0.000000000000000000 ) ) ;
#21197 = CARTESIAN_POINT ( 'NONE',  ( 10.00000000000000000, -3.974475837765555575, 92.41557521768190497 ) ) ;
#21198 = DIRECTION ( 'NONE',  ( 1.000000000000000000, -0.000000000000000000, -0.000000000000000000 ) ) ;
#21199 = EDGE_CURVE ( 'NONE', #14906, #6904, #368, .T. ) ;
#21200 = CYLINDRICAL_SURFACE ( 'NONE', #10142, 11.99999999999999645 ) ;
#21201 = EDGE_CURVE ( 'NONE', #13715, #17704, #2830, .T. ) ;
#21202 = CARTESIAN_POINT ( 'NONE',  ( 10.00000000000000000, -78.01214607583776228, 33.90124636420084414 ) ) ;
#21203 = EDGE_CURVE ( 'NONE', #2294, #1686, #12006, .T. ) ;
#21204 = VECTOR ( 'NONE', #5531, 1000.000000000000000 ) ;
#21205 = DIRECTION ( 'NONE',  ( -1.000000000000000000, -0.000000000000000000, -0.000000000000000000 ) ) ;
#21206 = DIRECTION ( 'NONE',  ( 0.000000000000000000, 0.7431448254773953543, -0.6691306063588569053 ) ) ;
#21207 = ADVANCED_FACE ( 'NONE', ( #5666 ), #4000, .T. ) ;
#21208 = PLANE ( 'NONE',  #19643 ) ;
#21209 = ORIENTED_EDGE ( 'NONE', *, *, #14901, .F. ) ;
#21210 = ORIENTED_EDGE ( 'NONE', *, *, #6689, .T. ) ;
#21211 = VERTEX_POINT ( 'NONE', #17814 ) ;
#21212 = EDGE_CURVE ( 'NONE', #11183, #5893, #6742, .T. ) ;
#21213 = ORIENTED_EDGE ( 'NONE', *, *, #9581, .F. ) ;
#21214 = VECTOR ( 'NONE', #3388, 1000.000000000000000 ) ;
#21215 = ORIENTED_EDGE ( 'NONE', *, *, #20662, .F. ) ;
#21216 = ADVANCED_FACE ( 'NONE', ( #14266 ), #6107, .F. ) ;
#21217 = CARTESIAN_POINT ( 'NONE',  ( 10.00000000000000000, 0.000000000000000000, 0.000000000000000000 ) ) ;
#21218 = VERTEX_POINT ( 'NONE', #15931 ) ;
#21219 = CARTESIAN_POINT ( 'NONE',  ( 0.000000000000000000, 41.21966518006070146, -82.80926399530243032 ) ) ;
#21220 = CARTESIAN_POINT ( 'NONE',  ( 0.000000000000000000, 0.000000000000000000, 0.000000000000000000 ) ) ;
#21221 = DIRECTION ( 'NONE',  ( 0.000000000000000000, -0.8987940462991619306, -0.4383711467890878399 ) ) ;
#21222 = CARTESIAN_POINT ( 'NONE',  ( 0.000000000000000000, 18.31866948046766552, 26.23788002993730828 ) ) ;
#21223 = DIRECTION ( 'NONE',  ( -1.000000000000000000, -0.000000000000000000, 0.000000000000000000 ) ) ;
#21224 = FACE_BOUND ( 'NONE', #15576, .T. ) ;
#21225 = EDGE_CURVE ( 'NONE', #13181, #19466, #13053, .T. ) ;
#21226 = DIRECTION ( 'NONE',  ( 1.000000000000000000, 0.000000000000000000, 0.000000000000000000 ) ) ;
#21227 = CYLINDRICAL_SURFACE ( 'NONE', #7485, 32.00000000000000000 ) ;
#21228 = DIRECTION ( 'NONE',  ( -1.000000000000000000, -0.000000000000000000, -0.000000000000000000 ) ) ;
#21229 = EDGE_CURVE ( 'NONE', #17490, #8447, #17658, .T. ) ;
#21230 = PRESENTATION_LAYER_ASSIGNMENT (  '', '', ( #17355 ) ) ;
#21231 = VERTEX_POINT ( 'NONE', #17928 ) ;
#21232 = DIRECTION ( 'NONE',  ( 0.000000000000000000, 0.000000000000000000, 1.000000000000000000 ) ) ;
#21233 = VERTEX_POINT ( 'NONE', #14384 ) ;
#21234 = CARTESIAN_POINT ( 'NONE',  ( -1.139999999999998570, 0.000000000000000000, 0.000000000000000000 ) ) ;
#21235 = ADVANCED_FACE ( 'NONE', ( #9283 ), #7648, .F. ) ;
#21236 = DIRECTION ( 'NONE',  ( -1.000000000000000000, 0.000000000000000000, 0.000000000000000000 ) ) ;
#21237 = ORIENTED_EDGE ( 'NONE', *, *, #3956, .T. ) ;
#21238 = CYLINDRICAL_SURFACE ( 'NONE', #3363, 44.99999999999999289 ) ;
#21239 = ORIENTED_EDGE ( 'NONE', *, *, #21076, .T. ) ;
#21240 = EDGE_CURVE ( 'NONE', #19614, #16153, #8480, .T. ) ;
#21241 = ORIENTED_EDGE ( 'NONE', *, *, #10681, .F. ) ;
#21242 = APPLICATION_PROTOCOL_DEFINITION ( 'draft international standard', 'automotive_design', 1998, #12070 ) ;
#21243 = DIRECTION ( 'NONE',  ( 0.000000000000000000, 0.2756373558169998295, -0.9612616959383187831 ) ) ;
#21244 = VERTEX_POINT ( 'NONE', #4117 ) ;
#21245 = ORIENTED_EDGE ( 'NONE', *, *, #14866, .T. ) ;
#21246 = EDGE_CURVE ( 'NONE', #3976, #15380, #21135, .T. ) ;
#21247 = CARTESIAN_POINT ( 'NONE',  ( 0.000000000000000000, 0.000000000000000000, -3.000000000000000000 ) ) ;
#21248 = CARTESIAN_POINT ( 'NONE',  ( 5.000000000000002665, 81.83745710415318797, -32.35167097270070258 ) ) ;
#21249 = EDGE_CURVE ( 'NONE', #9563, #12067, #11666, .T. ) ;
#21250 = DIRECTION ( 'NONE',  ( -1.000000000000000000, 0.000000000000000000, 0.000000000000000000 ) ) ;
#21251 = CARTESIAN_POINT ( 'NONE',  ( 0.000000000000000000, 0.000000000000000000, 0.000000000000000000 ) ) ;
#21252 = DIRECTION ( 'NONE',  ( -1.000000000000000000, -0.000000000000000000, -0.000000000000000000 ) ) ;
#21253 = DIRECTION ( 'NONE',  ( -1.000000000000000000, -0.000000000000000000, -0.000000000000000000 ) ) ;
#21254 = CARTESIAN_POINT ( 'NONE',  ( 10.00000000000000000, -15.25521607131190294, -23.70650506194185425 ) ) ;
#21255 = DIRECTION ( 'NONE',  ( 0.000000000000000000, 0.8290375725550390706, 0.5591929034707507906 ) ) ;
#21256 = CARTESIAN_POINT ( 'NONE',  ( 10.00000000000000000, 0.000000000000000000, 0.000000000000000000 ) ) ;
#21257 = AXIS2_PLACEMENT_3D ( 'NONE', #11871, #13961, #5249 ) ;
#21258 = EDGE_CURVE ( 'NONE', #6908, #2135, #1775, .T. ) ;
#21259 = ORIENTED_EDGE ( 'NONE', *, *, #10802, .T. ) ;
#21260 = CYLINDRICAL_SURFACE ( 'NONE', #18168, 88.00000000000000000 ) ;
#21261 = ORIENTED_EDGE ( 'NONE', *, *, #641, .T. ) ;
#21262 = DIRECTION ( 'NONE',  ( 0.000000000000000000, 0.000000000000000000, 1.000000000000000000 ) ) ;
#21263 = AXIS2_PLACEMENT_3D ( 'NONE', #7845, #14583, #1005 ) ;
#21264 = CARTESIAN_POINT ( 'NONE',  ( 0.000000000000000000, 57.53593069156372053, 72.42963261300981515 ) ) ;
#21265 = ORIENTED_EDGE ( 'NONE', *, *, #14464, .F. ) ;
#21266 = ORIENTED_EDGE ( 'NONE', *, *, #555, .T. ) ;
#21267 = EDGE_LOOP ( 'NONE', ( #6189, #7068, #5647, #17200 ) ) ;
#21268 = ORIENTED_EDGE ( 'NONE', *, *, #12665, .T. ) ;
#21269 = CARTESIAN_POINT ( 'NONE',  ( 7.395800000000001262, 0.000000000000000000, 0.000000000000000000 ) ) ;
#21270 = DIRECTION ( 'NONE',  ( 1.000000000000000000, 0.000000000000000000, 0.000000000000000000 ) ) ;
#21271 = AXIS2_PLACEMENT_3D ( 'NONE', #5387, #8706, #12016 ) ;
#21272 = EDGE_LOOP ( 'NONE', ( #1241, #9844, #10152, #18370 ) ) ;
#21273 = EDGE_CURVE ( 'NONE', #11293, #11232, #21018, .T. ) ;
#21274 = AXIS2_PLACEMENT_3D ( 'NONE', #573, #7321, #19127 ) ;
#21275 = DIRECTION ( 'NONE',  ( -3.552713678800500929E-15, 0.000000000000000000, 1.000000000000000000 ) ) ;
#21276 = CARTESIAN_POINT ( 'NONE',  ( 0.000000000000000000, 83.89484365856912973, 26.56417150042976161 ) ) ;
#21277 = CARTESIAN_POINT ( 'NONE',  ( 10.00000000000000000, -36.39558101400082535, -80.12091913260421450 ) ) ;
#21278 = CARTESIAN_POINT ( 'NONE',  ( 0.000000000000000000, 84.79630770241084292, -6.691460262315676033 ) ) ;
#21279 = DIRECTION ( 'NONE',  ( -1.000000000000000000, 0.000000000000000000, 0.000000000000000000 ) ) ;
#21280 = ORIENTED_EDGE ( 'NONE', *, *, #13948, .T. ) ;
#21281 = CARTESIAN_POINT ( 'NONE',  ( 10.00000000000000000, 39.87723064937119233, 83.46401306393586594 ) ) ;
#21282 = AXIS2_PLACEMENT_3D ( 'NONE', #15077, #11987, #10105 ) ;
#21283 = VECTOR ( 'NONE', #15896, 1000.000000000000000 ) ;
#21284 = CARTESIAN_POINT ( 'NONE',  ( 0.000000000000000000, 1.592605004253184964, -28.14575649959892445 ) ) ;
#21285 = ORIENTED_EDGE ( 'NONE', *, *, #18023, .F. ) ;
#21286 = CARTESIAN_POINT ( 'NONE',  ( 10.00000000000000000, -74.74361964203257003, 40.60271866773520344 ) ) ;
#21287 = ORIENTED_EDGE ( 'NONE', *, *, #8576, .T. ) ;
#21288 = CARTESIAN_POINT ( 'NONE',  ( 10.00000000000000000, 75.45728100697598961, 39.26051685139091063 ) ) ;
#21289 = ORIENTED_EDGE ( 'NONE', *, *, #10282, .F. ) ;
#21290 = CARTESIAN_POINT ( 'NONE',  ( 10.00000000000000000, -69.74988376403980794, -53.65588238863407611 ) ) ;
#21291 = AXIS2_PLACEMENT_3D ( 'NONE', #16112, #15994, #7725 ) ;
#21292 = ORIENTED_EDGE ( 'NONE', *, *, #19340, .T. ) ;
#21293 = ADVANCED_FACE ( 'NONE', ( #16365 ), #901, .F. ) ;
#21294 = VERTEX_POINT ( 'NONE', #21340 ) ;
#21295 = LINE ( 'NONE', #9564, #18531 ) ;
#21296 = ORIENTED_EDGE ( 'NONE', *, *, #16609, .F. ) ;
#21297 = LINE ( 'NONE', #19315, #4910 ) ;
#21298 = CIRCLE ( 'NONE', #11071, 0.2042000000000016025 ) ;
#21299 = DIRECTION ( 'NONE',  ( 0.000000000000000000, 0.000000000000000000, 1.000000000000000000 ) ) ;
#21300 = DIRECTION ( 'NONE',  ( 0.000000000000000000, 0.000000000000000000, 1.000000000000000000 ) ) ;
#21301 = CARTESIAN_POINT ( 'NONE',  ( 10.00000000000000000, 0.000000000000000000, 0.000000000000000000 ) ) ;
#21302 = EDGE_CURVE ( 'NONE', #18196, #13383, #10601, .T. ) ;
#21303 = VECTOR ( 'NONE', #13873, 1000.000000000000000 ) ;
#21304 = CYLINDRICAL_SURFACE ( 'NONE', #17190, 27.49900000000000233 ) ;
#21305 = DIRECTION ( 'NONE',  ( 0.000000000000000000, 0.000000000000000000, 1.000000000000000000 ) ) ;
#21306 = DIRECTION ( 'NONE',  ( -1.000000000000000000, -0.000000000000000000, 0.000000000000000000 ) ) ;
#21307 = CYLINDRICAL_SURFACE ( 'NONE', #12319, 88.00000000000000000 ) ;
#21308 = CIRCLE ( 'NONE', #21653, 92.50100000000000477 ) ;
#21309 = CARTESIAN_POINT ( 'NONE',  ( 10.00000000000000000, 0.000000000000000000, 0.000000000000000000 ) ) ;
#21310 = VECTOR ( 'NONE', #17833, 1000.000000000000000 ) ;
#21311 = ORIENTED_EDGE ( 'NONE', *, *, #9433, .T. ) ;
#21312 = ORIENTED_EDGE ( 'NONE', *, *, #782, .F. ) ;
#21313 = CIRCLE ( 'NONE', #11799, 5.453125000000000000 ) ;
#21314 = ORIENTED_EDGE ( 'NONE', *, *, #13110, .F. ) ;
#21315 = ORIENTED_EDGE ( 'NONE', *, *, #3634, .T. ) ;
#21316 = ADVANCED_FACE ( 'NONE', ( #1238 ), #14498, .T. ) ;
#21317 = ORIENTED_EDGE ( 'NONE', *, *, #6024, .T. ) ;
#21318 = DIRECTION ( 'NONE',  ( -1.000000000000000000, -0.000000000000000000, 0.000000000000000000 ) ) ;
#21319 = CIRCLE ( 'NONE', #2965, 92.50100000000000477 ) ;
#21320 = ORIENTED_EDGE ( 'NONE', *, *, #20032, .T. ) ;
#21321 = LINE ( 'NONE', #9705, #11724 ) ;
#21322 = CARTESIAN_POINT ( 'NONE',  ( 10.00000000000000000, 84.12297548659721258, 32.40974838672968872 ) ) ;
#21323 = CYLINDRICAL_SURFACE ( 'NONE', #1969, 44.99999999999998579 ) ;
#21324 = CARTESIAN_POINT ( 'NONE',  ( 0.000000000000000000, -14.02138820414970688, 83.89630571862279851 ) ) ;
#21325 = DIRECTION ( 'NONE',  ( -0.000000000000000000, 0.000000000000000000, 1.000000000000000000 ) ) ;
#21326 = CIRCLE ( 'NONE', #12488, 12.00000000000000000 ) ;
#21327 = DIRECTION ( 'NONE',  ( -1.000000000000000000, 0.000000000000000000, 0.000000000000000000 ) ) ;
#21328 = DIRECTION ( 'NONE',  ( -1.000000000000000000, -0.000000000000000000, -0.000000000000000000 ) ) ;
#21329 = EDGE_CURVE ( 'NONE', #11211, #9563, #20135, .T. ) ;
#21330 = CARTESIAN_POINT ( 'NONE',  ( -7.600000000000002309, 0.000000000000000000, 0.000000000000000000 ) ) ;
#21331 = VERTEX_POINT ( 'NONE', #17702 ) ;
#21332 = ADVANCED_FACE ( 'NONE', ( #11178 ), #16034, .T. ) ;
#21333 = CARTESIAN_POINT ( 'NONE',  ( -10.00000000000000000, 0.000000000000000000, 0.000000000000000000 ) ) ;
#21334 = CIRCLE ( 'NONE', #14262, 45.00000000000000711 ) ;
#21335 = AXIS2_PLACEMENT_3D ( 'NONE', #10942, #2537, #10616 ) ;
#21336 = VERTEX_POINT ( 'NONE', #19463 ) ;
#21337 = AXIS2_PLACEMENT_3D ( 'NONE', #21738, #8162, #6622 ) ;
#21338 = DIRECTION ( 'NONE',  ( 0.000000000000000000, 0.000000000000000000, 1.000000000000000000 ) ) ;
#21339 = CIRCLE ( 'NONE', #8999, 88.00000000000000000 ) ;
#21340 = CARTESIAN_POINT ( 'NONE',  ( 10.00000000000000000, -87.92084725184950855, 3.731570516142653116 ) ) ;
#21341 = EDGE_CURVE ( 'NONE', #1024, #18295, #16593, .T. ) ;
#21342 = EDGE_LOOP ( 'NONE', ( #6037, #11897, #21167, #20397 ) ) ;
#21343 = EDGE_CURVE ( 'NONE', #3351, #2769, #15888, .T. ) ;
#21344 = EDGE_CURVE ( 'NONE', #5130, #3522, #18373, .T. ) ;
#21345 = CYLINDRICAL_SURFACE ( 'NONE', #11233, 115.1000000000000227 ) ;
#21346 = ORIENTED_EDGE ( 'NONE', *, *, #18790, .F. ) ;
#21347 = EDGE_LOOP ( 'NONE', ( #15624, #17929, #8885, #7956 ) ) ;
#21348 = AXIS2_PLACEMENT_3D ( 'NONE', #14995, #16655, #6295 ) ;
#21349 = PRODUCT_CONTEXT ( 'NONE', #14765, 'mechanical' ) ;
#21350 = DIRECTION ( 'NONE',  ( 0.000000000000000000, 0.000000000000000000, 1.000000000000000000 ) ) ;
#21351 = EDGE_CURVE ( 'NONE', #15753, #3387, #21777, .T. ) ;
#21352 = ORIENTED_EDGE ( 'NONE', *, *, #702, .F. ) ;
#21353 = VERTEX_POINT ( 'NONE', #1349 ) ;
#21354 = CARTESIAN_POINT ( 'NONE',  ( 10.00000000000000000, -22.77465461094663368, -15.41136296218110147 ) ) ;
#21355 = CARTESIAN_POINT ( 'NONE',  ( 10.00000000000000000, -17.70753755129023332, -21.03896658273990639 ) ) ;
#21356 = FACE_OUTER_BOUND ( 'NONE', #6990, .T. ) ;
#21357 = DIRECTION ( 'NONE',  ( -1.000000000000000000, -0.000000000000000000, -0.000000000000000000 ) ) ;
#21358 = AXIS2_PLACEMENT_3D ( 'NONE', #16641, #13099, #3166 ) ;
#21359 = CARTESIAN_POINT ( 'NONE',  ( 10.00000000000000000, 0.000000000000000000, 0.000000000000000000 ) ) ;
#21360 = AXIS2_PLACEMENT_3D ( 'NONE', #7008, #8546, #5346 ) ;
#21361 = CARTESIAN_POINT ( 'NONE',  ( 10.00000000000000000, 0.000000000000000000, 0.000000000000000000 ) ) ;
#21362 = AXIS2_PLACEMENT_3D ( 'NONE', #14645, #13425, #6594 ) ;
#21363 = CARTESIAN_POINT ( 'NONE',  ( 10.00000000000000000, 0.000000000000000000, 0.000000000000000000 ) ) ;
#21364 = CARTESIAN_POINT ( 'NONE',  ( 0.000000000000000000, -35.18804927320584142, 80.65854690202667143 ) ) ;
#21365 = EDGE_CURVE ( 'NONE', #19161, #14453, #3894, .T. ) ;
#21367 = CIRCLE ( 'NONE', #7254, 12.00000000000000178 ) ;
#21366 = CYLINDRICAL_SURFACE ( 'NONE', #18972, 44.99999999999999289 ) ;
#21368 = ORIENTED_EDGE ( 'NONE', *, *, #13768, .T. ) ;
#21369 = EDGE_CURVE ( 'NONE', #10630, #18906, #2478, .T. ) ;
#21370 = FACE_OUTER_BOUND ( 'NONE', #495, .T. ) ;
#21371 = ORIENTED_EDGE ( 'NONE', *, *, #19605, .F. ) ;
#21372 = VECTOR ( 'NONE', #12980, 1000.000000000000000 ) ;
#21373 = EDGE_CURVE ( 'NONE', #18906, #20563, #23, .T. ) ;
#21374 = VECTOR ( 'NONE', #10401, 1000.000000000000000 ) ;
#21375 = DIRECTION ( 'NONE',  ( 0.000000000000000000, 0.000000000000000000, -1.000000000000000000 ) ) ;
#21376 =( NAMED_UNIT ( * ) PLANE_ANGLE_UNIT ( ) SI_UNIT ( $, .RADIAN. ) );
#21377 = AXIS2_PLACEMENT_3D ( 'NONE', #4551, #1017, #19679 ) ;
#21378 = CARTESIAN_POINT ( 'NONE',  ( 0.000000000000000000, 0.000000000000000000, 0.000000000000000000 ) ) ;
#21379 = CIRCLE ( 'NONE', #11850, 44.99999999999999289 ) ;
#21380 = ORIENTED_EDGE ( 'NONE', *, *, #3537, .F. ) ;
#21381 = VECTOR ( 'NONE', #21504, 1000.000000000000000 ) ;
#21382 = AXIS2_PLACEMENT_3D ( 'NONE', #5998, #19453, #14489 ) ;
#21383 = VERTEX_POINT ( 'NONE', #20130 ) ;
#21384 = ADVANCED_FACE ( 'NONE', ( #8521 ), #21667, .F. ) ;
#21385 = ORIENTED_EDGE ( 'NONE', *, *, #7436, .F. ) ;
#21386 = VERTEX_POINT ( 'NONE', #15244 ) ;
#21387 = CARTESIAN_POINT ( 'NONE',  ( 10.00000000000000000, -23.62010150527165919, -84.77081340225927875 ) ) ;
#21388 = DIRECTION ( 'NONE',  ( 0.000000000000000000, -6.982962677686266711E-15, 1.000000000000000000 ) ) ;
#21389 = ORIENTED_EDGE ( 'NONE', *, *, #14017, .F. ) ;
#21390 = DIRECTION ( 'NONE',  ( 0.000000000000000000, 0.000000000000000000, 1.000000000000000000 ) ) ;
#21391 = DIRECTION ( 'NONE',  ( 1.000000000000000000, 0.000000000000000000, 0.000000000000000000 ) ) ;
#21392 = DIRECTION ( 'NONE',  ( 0.000000000000000000, 0.000000000000000000, 1.000000000000000000 ) ) ;
#21393 = DIRECTION ( 'NONE',  ( -1.000000000000000000, -0.000000000000000000, -0.000000000000000000 ) ) ;
#21394 = CARTESIAN_POINT ( 'NONE',  ( 0.000000000000000000, 28.15804365424195765, 1.358152127006451826 ) ) ;
#21395 = VERTEX_POINT ( 'NONE', #13156 ) ;
#21396 = EDGE_CURVE ( 'NONE', #16625, #18856, #6338, .T. ) ;
#21397 = AXIS2_PLACEMENT_3D ( 'NONE', #9409, #19593, #14282 ) ;
#21398 = CARTESIAN_POINT ( 'NONE',  ( 10.00000000000000000, 0.000000000000000000, 0.000000000000000000 ) ) ;
#21399 = DIRECTION ( 'NONE',  ( 1.000000000000000000, 0.000000000000000000, 0.000000000000000000 ) ) ;
#21400 = EDGE_LOOP ( 'NONE', ( #17205, #10013, #14247, #18079 ) ) ;
#21401 = EDGE_CURVE ( 'NONE', #16630, #3522, #7420, .T. ) ;
#21402 = CYLINDRICAL_SURFACE ( 'NONE', #16134, 44.99999999999999289 ) ;
#21403 = ORIENTED_EDGE ( 'NONE', *, *, #7705, .F. ) ;
#21404 = DIRECTION ( 'NONE',  ( 1.000000000000000000, 0.000000000000000000, 0.000000000000000000 ) ) ;
#21405 = DIRECTION ( 'NONE',  ( 0.000000000000000000, 0.000000000000000000, 1.000000000000000000 ) ) ;
#21406 = VERTEX_POINT ( 'NONE', #4659 ) ;
#21407 = CARTESIAN_POINT ( 'NONE',  ( 10.00000000000000000, -4.294029059349679045, -27.86182539015970505 ) ) ;
#21408 = VERTEX_POINT ( 'NONE', #4987 ) ;
#21409 = AXIS2_PLACEMENT_3D ( 'NONE', #2143, #8876, #20278 ) ;
#21410 = VERTEX_POINT ( 'NONE', #8192 ) ;
#21411 = DIRECTION ( 'NONE',  ( 0.000000000000000000, 0.000000000000000000, 1.000000000000000000 ) ) ;
#21412 = ORIENTED_EDGE ( 'NONE', *, *, #13673, .T. ) ;
#21413 = CYLINDRICAL_SURFACE ( 'NONE', #8098, 11.99999999999999822 ) ;
#21414 = CARTESIAN_POINT ( 'NONE',  ( 0.000000000000000000, 0.000000000000000000, 15.00000000000000000 ) ) ;
#21415 = CARTESIAN_POINT ( 'NONE',  ( -10.00000000000000000, 0.000000000000000000, 0.000000000000000000 ) ) ;
#21416 = CARTESIAN_POINT ( 'NONE',  ( 10.00000000000000000, 0.000000000000000000, 0.000000000000000000 ) ) ;
#21417 = LINE ( 'NONE', #13021, #6631 ) ;
#21418 = CARTESIAN_POINT ( 'NONE',  ( 10.00000000000000000, 0.000000000000000000, 0.000000000000000000 ) ) ;
#21419 = DIRECTION ( 'NONE',  ( 0.000000000000000000, 0.5299192642332061221, -0.8480480961564251796 ) ) ;
#21420 = DIRECTION ( 'NONE',  ( -1.000000000000000000, -0.000000000000000000, -0.000000000000000000 ) ) ;
#21421 = CIRCLE ( 'NONE', #14709, 44.99999999999999289 ) ;
#21422 = DIRECTION ( 'NONE',  ( 0.000000000000000000, 0.000000000000000000, -1.000000000000000000 ) ) ;
#21423 = AXIS2_PLACEMENT_3D ( 'NONE', #634, #7065, #7385 ) ;
#21424 = AXIS2_PLACEMENT_3D ( 'NONE', #7294, #14020, #20768 ) ;
#21425 = CARTESIAN_POINT ( 'NONE',  ( 10.00000000000000000, 4.294029059349855793, 27.86182539015968018 ) ) ;
#21426 = ORIENTED_EDGE ( 'NONE', *, *, #10707, .T. ) ;
#21427 = ORIENTED_EDGE ( 'NONE', *, *, #8300, .F. ) ;
#21428 = ORIENTED_EDGE ( 'NONE', *, *, #549, .F. ) ;
#21429 = ORIENTED_EDGE ( 'NONE', *, *, #16247, .F. ) ;
#21430 = ORIENTED_EDGE ( 'NONE', *, *, #19343, .F. ) ;
#21431 = DIRECTION ( 'NONE',  ( -1.000000000000000000, -0.000000000000000000, -0.000000000000000000 ) ) ;
#21432 = AXIS2_PLACEMENT_3D ( 'NONE', #3078, #19867, #14564 ) ;
#21433 = ORIENTED_EDGE ( 'NONE', *, *, #11162, .T. ) ;
#21434 = DIRECTION ( 'NONE',  ( 0.000000000000000000, 0.06975647374411846069, 0.9975640502598246417 ) ) ;
#21435 = AXIS2_PLACEMENT_3D ( 'NONE', #20828, #4252, #5690 ) ;
#21436 = AXIS2_PLACEMENT_3D ( 'NONE', #6738, #86, #12015 ) ;
#21437 = CARTESIAN_POINT ( 'NONE',  ( 10.00000000000000000, -3.728035544475628793, -84.97818067823773447 ) ) ;
#21438 = AXIS2_PLACEMENT_3D ( 'NONE', #1010, #12386, #779 ) ;
#21439 = DIRECTION ( 'NONE',  ( 0.000000000000000000, 0.000000000000000000, 1.000000000000000000 ) ) ;
#21440 = CARTESIAN_POINT ( 'NONE',  ( 10.00000000000000000, 72.58367602204255320, -49.75550195834793499 ) ) ;
#21441 = DIRECTION ( 'NONE',  ( -1.000000000000000000, 0.000000000000000000, 0.000000000000000000 ) ) ;
#21442 = DIRECTION ( 'NONE',  ( 0.000000000000000000, 0.000000000000000000, 1.000000000000000000 ) ) ;
#21443 = DIRECTION ( 'NONE',  ( 1.000000000000000000, -0.000000000000000000, -0.000000000000000000 ) ) ;
#21444 = EDGE_CURVE ( 'NONE', #15380, #4970, #6382, .T. ) ;
#21445 = ORIENTED_EDGE ( 'NONE', *, *, #21229, .F. ) ;
#21446 = FACE_OUTER_BOUND ( 'NONE', #1187, .T. ) ;
#21447 = AXIS2_PLACEMENT_3D ( 'NONE', #1567, #13605, #8099 ) ;
#21448 = AXIS2_PLACEMENT_3D ( 'NONE', #5789, #10861, #7663 ) ;
#21449 = AXIS2_PLACEMENT_3D ( 'NONE', #19137, #12291, #3895 ) ;
#21450 = CIRCLE ( 'NONE', #15461, 120.0000000000000000 ) ;
#21451 = ORIENTED_EDGE ( 'NONE', *, *, #15301, .T. ) ;
#21452 = AXIS2_PLACEMENT_3D ( 'NONE', #468, #13732, #20254 ) ;
#21453 = ADVANCED_FACE ( 'NONE', ( #11394 ), #16479, .F. ) ;
#21454 = ORIENTED_EDGE ( 'NONE', *, *, #12198, .F. ) ;
#21455 = DIRECTION ( 'NONE',  ( -1.000000000000000000, 0.000000000000000000, -0.000000000000000000 ) ) ;
#21456 = DIRECTION ( 'NONE',  ( -1.000000000000000000, -0.000000000000000000, -0.000000000000000000 ) ) ;
#21457 = ORIENTED_EDGE ( 'NONE', *, *, #9178, .F. ) ;
#21458 = CARTESIAN_POINT ( 'NONE',  ( 5.000000000000002665, -0.6609040254605889064, -87.99751818016876825 ) ) ;
#21459 = VERTEX_POINT ( 'NONE', #14928 ) ;
#21460 = EDGE_LOOP ( 'NONE', ( #3443, #18233, #1509, #12375 ) ) ;
#21461 = APPLICATION_PROTOCOL_DEFINITION ( 'draft international standard', 'automotive_design', 1998, #14765 ) ;
#21462 = CIRCLE ( 'NONE', #14762, 88.00000000000000000 ) ;
#21463 = EDGE_CURVE ( 'NONE', #16306, #4799, #5315, .T. ) ;
#21464 = CARTESIAN_POINT ( 'NONE',  ( 0.000000000000000000, -78.80192417387900150, -39.16958956249377621 ) ) ;
#21465 = ORIENTED_EDGE ( 'NONE', *, *, #13948, .F. ) ;
#21466 = ORIENTED_EDGE ( 'NONE', *, *, #12945, .T. ) ;
#21467 = DIRECTION ( 'NONE',  ( 0.000000000000000000, 0.000000000000000000, 1.000000000000000000 ) ) ;
#21468 = DIRECTION ( 'NONE',  ( 1.000000000000000000, 0.000000000000000000, -0.000000000000000000 ) ) ;
#21469 = AXIS2_PLACEMENT_3D ( 'NONE', #3422, #8072, #16460 ) ;
#21470 = CARTESIAN_POINT ( 'NONE',  ( 10.00000000000000000, 0.000000000000000000, 0.000000000000000000 ) ) ;
#21471 = CARTESIAN_POINT ( 'NONE',  ( 10.00000000000000000, -56.35896156214997887, 73.34918167666290856 ) ) ;
#21472 = AXIS2_PLACEMENT_3D ( 'NONE', #6221, #9609, #5075 ) ;
#21473 = DIRECTION ( 'NONE',  ( 0.000000000000000000, 0.000000000000000000, 1.000000000000000000 ) ) ;
#21474 = AXIS2_PLACEMENT_3D ( 'NONE', #14603, #1562, #16485 ) ;
#21475 = DIRECTION ( 'NONE',  ( -1.000000000000000000, -0.000000000000000000, 0.000000000000000000 ) ) ;
#21476 = CIRCLE ( 'NONE', #7363, 92.50100000000000477 ) ;
#21477 = CYLINDRICAL_SURFACE ( 'NONE', #7539, 92.50100000000000477 ) ;
#21478 = DIRECTION ( 'NONE',  ( 0.000000000000000000, 0.000000000000000000, 1.000000000000000000 ) ) ;
#21479 = LINE ( 'NONE', #13071, #6646 ) ;
#21480 = ADVANCED_FACE ( 'NONE', ( #16591 ), #3000, .T. ) ;
#21481 = EDGE_CURVE ( 'NONE', #481, #11418, #5328, .T. ) ;
#21482 = ADVANCED_FACE ( 'NONE', ( #15146 ), #21, .F. ) ;
#21483 = ORIENTED_EDGE ( 'NONE', *, *, #14153, .F. ) ;
#21484 = EDGE_CURVE ( 'NONE', #12477, #3300, #5212, .T. ) ;
#21485 = ORIENTED_EDGE ( 'NONE', *, *, #17448, .F. ) ;
#21486 = CARTESIAN_POINT ( 'NONE',  ( 10.00000000000000000, 79.66702613806732813, 29.80527447819576636 ) ) ;
#21487 = AXIS2_PLACEMENT_3D ( 'NONE', #12034, #7076, #10264 ) ;
#21488 = DIRECTION ( 'NONE',  ( 0.000000000000000000, 0.000000000000000000, 1.000000000000000000 ) ) ;
#21489 = AXIS2_PLACEMENT_3D ( 'NONE', #18427, #6823, #16646 ) ;
#21490 = CIRCLE ( 'NONE', #12303, 92.50100000000003320 ) ;
#21491 = DIRECTION ( 'NONE',  ( 0.000000000000000000, 0.9510565162951544194, -0.3090169943749448977 ) ) ;
#21492 = CIRCLE ( 'NONE', #3843, 44.99999999999999289 ) ;
#21493 = ORIENTED_EDGE ( 'NONE', *, *, #837, .F. ) ;
#21494 = EDGE_CURVE ( 'NONE', #20304, #301, #6871, .T. ) ;
#21495 = ORIENTED_EDGE ( 'NONE', *, *, #13831, .T. ) ;
#21496 = ORIENTED_EDGE ( 'NONE', *, *, #15358, .T. ) ;
#21497 = ORIENTED_EDGE ( 'NONE', *, *, #5326, .F. ) ;
#21498 = CARTESIAN_POINT ( 'NONE',  ( 0.000000000000000000, 46.93287725819874368, -70.94007663282398823 ) ) ;
#21499 = CARTESIAN_POINT ( 'NONE',  ( 10.00000000000000000, 0.000000000000000000, 0.000000000000000000 ) ) ;
#21500 = VERTEX_POINT ( 'NONE', #9055 ) ;
#21501 = EDGE_CURVE ( 'NONE', #20567, #11727, #5664, .T. ) ;
#21502 = DIRECTION ( 'NONE',  ( 0.000000000000000000, 0.06975647374412555224, -0.9975640502598241977 ) ) ;
#21503 = DIRECTION ( 'NONE',  ( -1.000000000000000000, -0.000000000000000000, -0.000000000000000000 ) ) ;
#21504 = DIRECTION ( 'NONE',  ( -1.000000000000000000, 0.000000000000000000, 0.000000000000000000 ) ) ;
#21505 = DIRECTION ( 'NONE',  ( 1.000000000000000000, 0.000000000000000000, 0.000000000000000000 ) ) ;
#21506 = DIRECTION ( 'NONE',  ( 0.000000000000000000, 0.000000000000000000, 1.000000000000000000 ) ) ;
#21507 = CARTESIAN_POINT ( 'NONE',  ( -6.500000000000014211, 60.00000000000001421, -3.000000000000000000 ) ) ;
#21508 = AXIS2_PLACEMENT_3D ( 'NONE', #10455, #3506, #15314 ) ;
#21509 = AXIS2_PLACEMENT_3D ( 'NONE', #931, #12532, #4145 ) ;
#21510 = AXIS2_PLACEMENT_3D ( 'NONE', #11780, #13435, #13209 ) ;
#21511 = ORIENTED_EDGE ( 'NONE', *, *, #6379, .F. ) ;
#21512 = AXIS2_PLACEMENT_3D ( 'NONE', #15882, #19087, #17756 ) ;
#21513 = CARTESIAN_POINT ( 'NONE',  ( 7.440711023145912151, 1.285874240517524538E-14, 104.9000000000000341 ) ) ;
#21514 = ADVANCED_FACE ( 'NONE', ( #14030 ), #20780, .F. ) ;
#21515 = CARTESIAN_POINT ( 'NONE',  ( 0.000000000000000000, -87.58454185039434492, -8.540961822682595184 ) ) ;
#21516 = VERTEX_POINT ( 'NONE', #15362 ) ;
#21517 = DIRECTION ( 'NONE',  ( 0.000000000000000000, 0.000000000000000000, 1.000000000000000000 ) ) ;
#21518 = VERTEX_POINT ( 'NONE', #13716 ) ;
#21519 = CARTESIAN_POINT ( 'NONE',  ( 10.00000000000000000, -85.54350296776125617, 20.64725405482824883 ) ) ;
#21520 = DIRECTION ( 'NONE',  ( 1.000000000000000000, 0.000000000000000000, 0.000000000000000000 ) ) ;
#21521 = EDGE_LOOP ( 'NONE', ( #3765, #18354, #6490, #21524 ) ) ;
#21522 = CARTESIAN_POINT ( 'NONE',  ( 0.000000000000000000, 78.01214607583800387, -33.90124636420030413 ) ) ;
#21523 = EDGE_CURVE ( 'NONE', #2135, #3522, #10716, .T. ) ;
#21524 = ORIENTED_EDGE ( 'NONE', *, *, #4741, .T. ) ;
#21525 = ORIENTED_EDGE ( 'NONE', *, *, #17712, .F. ) ;
#21526 = VECTOR ( 'NONE', #4911, 1000.000000000000000 ) ;
#21527 = LINE ( 'NONE', #16551, #6237 ) ;
#21528 = EDGE_CURVE ( 'NONE', #1002, #5874, #5429, .T. ) ;
#21529 = ORIENTED_EDGE ( 'NONE', *, *, #7315, .T. ) ;
#21530 = DIRECTION ( 'NONE',  ( 0.000000000000000000, 0.000000000000000000, 1.000000000000000000 ) ) ;
#21531 = CARTESIAN_POINT ( 'NONE',  ( 10.00000000000000000, 12.94633825542301153, -24.26081875733320814 ) ) ;
#21532 = FACE_OUTER_BOUND ( 'NONE', #1738, .T. ) ;
#21533 = EDGE_CURVE ( 'NONE', #19231, #16476, #17026, .T. ) ;
#21534 = EDGE_CURVE ( 'NONE', #2262, #11402, #13072, .T. ) ;
#21535 = CARTESIAN_POINT ( 'NONE',  ( 10.00000000000000000, 17.64925110578583300, -86.21197095186326464 ) ) ;
#21536 = DIRECTION ( 'NONE',  ( 0.000000000000000000, 0.000000000000000000, 1.000000000000000000 ) ) ;
#21537 = DIRECTION ( 'NONE',  ( 0.000000000000000000, 0.000000000000000000, 1.000000000000000000 ) ) ;
#21538 = DIRECTION ( 'NONE',  ( 0.000000000000000000, 0.4067366430757947127, 0.9135454576426031981 ) ) ;
#21539 = LINE ( 'NONE', #3410, #3345 ) ;
#21540 = AXIS2_PLACEMENT_3D ( 'NONE', #19903, #13051, #19797 ) ;
#21541 = DIRECTION ( 'NONE',  ( 0.000000000000000000, 0.000000000000000000, 1.000000000000000000 ) ) ;
#21542 = ORIENTED_EDGE ( 'NONE', *, *, #2843, .T. ) ;
#21543 = VERTEX_POINT ( 'NONE', #122 ) ;
#21544 = VERTEX_POINT ( 'NONE', #1884 ) ;
#21545 = ORIENTED_EDGE ( 'NONE', *, *, #45, .F. ) ;
#21546 = EDGE_LOOP ( 'NONE', ( #11329, #7027, #9118, #13575, #260, #2133 ) ) ;
#21547 = FACE_OUTER_BOUND ( 'NONE', #11034, .T. ) ;
#21548 = ORIENTED_EDGE ( 'NONE', *, *, #11598, .F. ) ;
#21549 = CYLINDRICAL_SURFACE ( 'NONE', #6803, 92.50100000000000477 ) ;
#21550 = CIRCLE ( 'NONE', #9542, 12.00000000000000000 ) ;
#21551 = CARTESIAN_POINT ( 'NONE',  ( 10.00000000000000000, -27.26034713664092379, 4.817140289263571518 ) ) ;
#21552 = CARTESIAN_POINT ( 'NONE',  ( 0.000000000000000000, -21.69483248597433089, 16.89761061231773454 ) ) ;
#21553 = FACE_OUTER_BOUND ( 'NONE', #21756, .T. ) ;
#21554 = CARTESIAN_POINT ( 'NONE',  ( -10.00000000000000000, 0.000000000000000000, 0.000000000000000000 ) ) ;
#21555 = CARTESIAN_POINT ( 'NONE',  ( 10.00000000000000000, 0.000000000000000000, 0.000000000000000000 ) ) ;
#21556 = CARTESIAN_POINT ( 'NONE',  ( 0.000000000000000000, 75.45728100697654384, -39.26051685138985903 ) ) ;
#21557 = AXIS2_PLACEMENT_3D ( 'NONE', #1494, #13315, #1721 ) ;
#21558 = ORIENTED_EDGE ( 'NONE', *, *, #12001, .T. ) ;
#21559 = CARTESIAN_POINT ( 'NONE',  ( -10.00000000000000000, 0.000000000000000000, 0.000000000000000000 ) ) ;
#21560 = STYLED_ITEM ( 'NONE', ( #13079 ), #7762 ) ;
#21561 = ORIENTED_EDGE ( 'NONE', *, *, #18702, .F. ) ;
#21562 = ORIENTED_EDGE ( 'NONE', *, *, #21748, .T. ) ;
#21563 = DIRECTION ( 'NONE',  ( -1.000000000000000000, 0.000000000000000000, -0.000000000000000000 ) ) ;
#21564 = VERTEX_POINT ( 'NONE', #20467 ) ;
#21565 = FACE_OUTER_BOUND ( 'NONE', #16548, .T. ) ;
#21566 = VERTEX_POINT ( 'NONE', #13600 ) ;
#21567 = ORIENTED_EDGE ( 'NONE', *, *, #8798, .T. ) ;
#21568 = EDGE_CURVE ( 'NONE', #20538, #19711, #14131, .T. ) ;
#21569 = APPLICATION_PROTOCOL_DEFINITION ( 'draft international standard', 'automotive_design', 1998, #1204 ) ;
#21570 = CARTESIAN_POINT ( 'NONE',  ( 0.000000000000000000, -27.00677879428973682, -80.65868421664460186 ) ) ;
#21571 = ORIENTED_EDGE ( 'NONE', *, *, #1275, .F. ) ;
#21572 = EDGE_CURVE ( 'NONE', #13306, #2453, #16611, .T. ) ;
#21573 = DIRECTION ( 'NONE',  ( 1.000000000000000000, 0.000000000000000000, 0.000000000000000000 ) ) ;
#21574 = DIRECTION ( 'NONE',  ( -1.000000000000000000, 0.000000000000000000, -0.000000000000000000 ) ) ;
#21575 = CARTESIAN_POINT ( 'NONE',  ( 0.000000000000000000, 27.40684453873989668, -16.51862198941980608 ) ) ;
#21576 = DIRECTION ( 'NONE',  ( -1.000000000000000000, 0.000000000000000000, 0.000000000000000000 ) ) ;
#21577 = STYLED_ITEM ( 'NONE', ( #20267 ), #6478 ) ;
#21578 = DIRECTION ( 'NONE',  ( -1.000000000000000000, 0.000000000000000000, -0.000000000000000000 ) ) ;
#21579 = ADVANCED_FACE ( 'NONE', ( #3764 ), #12264, .F. ) ;
#21580 = DIRECTION ( 'NONE',  ( -1.000000000000000000, -0.000000000000000000, -0.000000000000000000 ) ) ;
#21581 = DIRECTION ( 'NONE',  ( 0.000000000000000000, 0.000000000000000000, 1.000000000000000000 ) ) ;
#21582 = LINE ( 'NONE', #6459, #1698 ) ;
#21583 = VERTEX_POINT ( 'NONE', #19118 ) ;
#21584 = LINE ( 'NONE', #4797, #10845 ) ;
#21585 = DIRECTION ( 'NONE',  ( 0.000000000000000000, 0.5877852522924690293, 0.8090169943749504489 ) ) ;
#21586 = ORIENTED_EDGE ( 'NONE', *, *, #18957, .T. ) ;
#21587 = CARTESIAN_POINT ( 'NONE',  ( 0.000000000000000000, -60.65279801375385915, 63.75921967137595914 ) ) ;
#21588 = VERTEX_POINT ( 'NONE', #13923 ) ;
#21589 = EDGE_LOOP ( 'NONE', ( #5014, #2158, #8674, #11458 ) ) ;
#21590 = DIRECTION ( 'NONE',  ( 1.000000000000000000, 0.000000000000000000, 0.000000000000000000 ) ) ;
#21591 = ORIENTED_EDGE ( 'NONE', *, *, #10146, .T. ) ;
#21592 = EDGE_CURVE ( 'NONE', #1543, #13950, #15198, .T. ) ;
#21593 = EDGE_CURVE ( 'NONE', #75, #5185, #3877, .T. ) ;
#21594 = VERTEX_POINT ( 'NONE', #17143 ) ;
#21595 = DIRECTION ( 'NONE',  ( -1.000000000000000000, -0.000000000000000000, -0.000000000000000000 ) ) ;
#21596 = DIRECTION ( 'NONE',  ( 1.000000000000000000, 0.000000000000000000, 0.000000000000000000 ) ) ;
#21597 = VERTEX_POINT ( 'NONE', #3978 ) ;
#21598 = LINE ( 'NONE', #14963, #15696 ) ;
#21599 = CARTESIAN_POINT ( 'NONE',  ( 10.00000000000000000, 21.69483248597422076, 16.89761061231787309 ) ) ;
#21600 = DIRECTION ( 'NONE',  ( 1.000000000000000000, -0.000000000000000000, -0.000000000000000000 ) ) ;
#21601 = CARTESIAN_POINT ( 'NONE',  ( 120.0000000000000000, 0.000000000000000000, 25.00000000000000000 ) ) ;
#21602 = CARTESIAN_POINT ( 'NONE',  ( 10.00000000000000000, 3.786343810537573518, 27.23708136986054029 ) ) ;
#21603 = DIRECTION ( 'NONE',  ( -1.000000000000000000, 0.000000000000000000, 0.000000000000000000 ) ) ;
#21604 = ORIENTED_EDGE ( 'NONE', *, *, #5736, .F. ) ;
#21605 = DIRECTION ( 'NONE',  ( 1.000000000000000000, 0.000000000000000000, 0.000000000000000000 ) ) ;
#21606 = EDGE_CURVE ( 'NONE', #7135, #874, #3551, .T. ) ;
#21607 = AXIS2_PLACEMENT_3D ( 'NONE', #460, #5762, #19237 ) ;
#21608 = CARTESIAN_POINT ( 'NONE',  ( 0.000000000000000000, 64.66851233300727131, 55.25552418572984692 ) ) ;
#21609 = ORIENTED_EDGE ( 'NONE', *, *, #7315, .F. ) ;
#21610 = ADVANCED_FACE ( 'NONE', ( #2210 ), #8945, .F. ) ;
#21611 = FACE_OUTER_BOUND ( 'NONE', #4807, .T. ) ;
#21612 = ORIENTED_EDGE ( 'NONE', *, *, #10758, .F. ) ;
#21613 = CARTESIAN_POINT ( 'NONE',  ( 10.00000000000000000, -86.54587337002888603, 15.93147207946976707 ) ) ;
#21614 = DIRECTION ( 'NONE',  ( 0.000000000000000000, 0.000000000000000000, 1.000000000000000000 ) ) ;
#21615 = ORIENTED_EDGE ( 'NONE', *, *, #15442, .F. ) ;
#21616 = CARTESIAN_POINT ( 'NONE',  ( 0.000000000000000000, 15.25521607131237722, -23.70650506194154872 ) ) ;
#21618 = EDGE_CURVE ( 'NONE', #6116, #13273, #2492, .T. ) ;
#21617 = ORIENTED_EDGE ( 'NONE', *, *, #20544, .F. ) ;
#21619 = EDGE_CURVE ( 'NONE', #16625, #12763, #19429, .T. ) ;
#21620 = ORIENTED_EDGE ( 'NONE', *, *, #10310, .F. ) ;
#21621 = EDGE_CURVE ( 'NONE', #19781, #616, #2947, .T. ) ;
#21622 = DIRECTION ( 'NONE',  ( -1.000000000000000000, 0.000000000000000000, 0.000000000000000000 ) ) ;
#21623 = ORIENTED_EDGE ( 'NONE', *, *, #2167, .T. ) ;
#21624 = CYLINDRICAL_SURFACE ( 'NONE', #8445, 3.000000000000000444 ) ;
#21625 = EDGE_CURVE ( 'NONE', #4602, #13330, #9903, .T. ) ;
#21626 = DIRECTION ( 'NONE',  ( 0.000000000000000000, 0.9848077530122085754, -0.1736481776669272226 ) ) ;
#21627 = DIRECTION ( 'NONE',  ( 1.000000000000000000, 0.000000000000000000, 0.000000000000000000 ) ) ;
#21628 = DIRECTION ( 'NONE',  ( 0.000000000000000000, 0.000000000000000000, 1.000000000000000000 ) ) ;
#21629 = DIRECTION ( 'NONE',  ( 0.000000000000000000, 0.000000000000000000, 1.000000000000000000 ) ) ;
#21630 = CIRCLE ( 'NONE', #20216, 92.50100000000000477 ) ;
#21631 = FACE_OUTER_BOUND ( 'NONE', #9134, .T. ) ;
#21632 = DIRECTION ( 'NONE',  ( -1.000000000000000000, 0.000000000000000000, -0.000000000000000000 ) ) ;
#21633 = AXIS2_PLACEMENT_3D ( 'NONE', #5243, #6905, #20160 ) ;
#21634 = CARTESIAN_POINT ( 'NONE',  ( 10.00000000000000000, -81.83745710415297481, 32.35167097270122838 ) ) ;
#21635 = EDGE_CURVE ( 'NONE', #16691, #2943, #8494, .T. ) ;
#21636 = DIRECTION ( 'NONE',  ( 1.000000000000000000, 0.000000000000000000, 0.000000000000000000 ) ) ;
#21637 = EDGE_CURVE ( 'NONE', #1263, #6576, #11341, .T. ) ;
#21638 = DIRECTION ( 'NONE',  ( 0.000000000000000000, 0.4694715627858916940, -0.8829475928589264333 ) ) ;
#21639 = ORIENTED_EDGE ( 'NONE', *, *, #3334, .T. ) ;
#21640 = AXIS2_PLACEMENT_3D ( 'NONE', #20977, #7823, #5852 ) ;
#21641 = ORIENTED_EDGE ( 'NONE', *, *, #1122, .F. ) ;
#21642 = ADVANCED_FACE ( 'NONE', ( #9789 ), #17993, .F. ) ;
#21643 = ORIENTED_EDGE ( 'NONE', *, *, #641, .F. ) ;
#21644 = AXIS2_PLACEMENT_3D ( 'NONE', #9991, #16735, #1606 ) ;
#21645 = VERTEX_POINT ( 'NONE', #21290 ) ;
#21646 = AXIS2_PLACEMENT_3D ( 'NONE', #4664, #19368, #11072 ) ;
#21647 = ORIENTED_EDGE ( 'NONE', *, *, #14210, .F. ) ;
#21648 = CARTESIAN_POINT ( 'NONE',  ( 10.00000000000000000, -27.87320266523616752, 88.20158487341750231 ) ) ;
#21649 = EDGE_CURVE ( 'NONE', #19231, #7150, #10252, .T. ) ;
#21650 = ORIENTED_EDGE ( 'NONE', *, *, #15435, .T. ) ;
#21651 = CARTESIAN_POINT ( 'NONE',  ( 10.00000000000000000, -28.00896854772001987, 15.47571261340913473 ) ) ;
#21652 = LINE ( 'NONE', #21551, #17038 ) ;
#21653 = AXIS2_PLACEMENT_3D ( 'NONE', #4374, #9125, #11114 ) ;
#21654 = FACE_OUTER_BOUND ( 'NONE', #15094, .T. ) ;
#21655 = CYLINDRICAL_SURFACE ( 'NONE', #20074, 88.00000000000000000 ) ;
#21656 = DIRECTION ( 'NONE',  ( -1.000000000000000000, 0.000000000000000000, 0.000000000000000000 ) ) ;
#21657 = CARTESIAN_POINT ( 'NONE',  ( 10.00000000000000000, -2.481790431839894673, 92.46770094066590673 ) ) ;
#21658 = CARTESIAN_POINT ( 'NONE',  ( 10.00000000000000000, -8.925965667928249303, -92.06933331948791022 ) ) ;
#21659 = AXIS2_PLACEMENT_3D ( 'NONE', #16709, #18715, #6686 ) ;
#21660 = ORIENTED_EDGE ( 'NONE', *, *, #14627, .F. ) ;
#21661 = ADVANCED_FACE ( 'NONE', ( #668, #13214 ), #14445, .T. ) ;
#21662 = VECTOR ( 'NONE', #3149, 1000.000000000000000 ) ;
#21663 = DIRECTION ( 'NONE',  ( 0.000000000000000000, -0.8660254037844328234, -0.5000000000000101030 ) ) ;
#21664 = VERTEX_POINT ( 'NONE', #19851 ) ;
#21665 = EDGE_CURVE ( 'NONE', #5595, #11788, #21550, .T. ) ;
#21666 = ORIENTED_EDGE ( 'NONE', *, *, #21619, .T. ) ;
#21667 = CYLINDRICAL_SURFACE ( 'NONE', #14480, 45.00000000000000000 ) ;
#21668 = VECTOR ( 'NONE', #1169, 1000.000000000000000 ) ;
#21669 = ORIENTED_EDGE ( 'NONE', *, *, #13640, .T. ) ;
#21670 = DIRECTION ( 'NONE',  ( 0.000000000000000000, 1.850371707708594760E-15, -1.000000000000000000 ) ) ;
#21671 = ORIENTED_EDGE ( 'NONE', *, *, #851, .T. ) ;
#21672 = ORIENTED_EDGE ( 'NONE', *, *, #13881, .T. ) ;
#21673 = APPLICATION_PROTOCOL_DEFINITION ( 'draft international standard', 'automotive_design', 1998, #1631 ) ;
#21674 = CIRCLE ( 'NONE', #14970, 7.500000000000000000 ) ;
#21675 = FACE_OUTER_BOUND ( 'NONE', #21729, .T. ) ;
#21676 = VERTEX_POINT ( 'NONE', #19751 ) ;
#21677 = LINE ( 'NONE', #6566, #174 ) ;
#21678 = VECTOR ( 'NONE', #19147, 1000.000000000000000 ) ;
#21679 = DIRECTION ( 'NONE',  ( -1.000000000000000000, 0.000000000000000000, -0.000000000000000000 ) ) ;
#21680 = CARTESIAN_POINT ( 'NONE',  ( 10.00000000000000000, 0.000000000000000000, 0.000000000000000000 ) ) ;
#21681 = FACE_BOUND ( 'NONE', #13358, .T. ) ;
#21682 = FACE_OUTER_BOUND ( 'NONE', #21347, .T. ) ;
#21683 = CARTESIAN_POINT ( 'NONE',  ( 0.000000000000000000, 0.000000000000000000, 0.000000000000000000 ) ) ;
#21684 = FACE_BOUND ( 'NONE', #9748, .T. ) ;
#21685 = CARTESIAN_POINT ( 'NONE',  ( 10.00000000000000000, 80.18694381077108346, 28.37681241246682973 ) ) ;
#21686 = AXIS2_PLACEMENT_3D ( 'NONE', #10831, #7201, #772 ) ;
#21687 = ORIENTED_EDGE ( 'NONE', *, *, #7645, .T. ) ;
#21688 = AXIS2_PLACEMENT_3D ( 'NONE', #12805, #16557, #21628 ) ;
#21690 = AXIS2_PLACEMENT_3D ( 'NONE', #10196, #1801, #17043 ) ;
#21689 = AXIS2_PLACEMENT_3D ( 'NONE', #19052, #9195, #5466 ) ;
#21691 = VECTOR ( 'NONE', #8724, 1000.000000000000000 ) ;
#21692 = DIRECTION ( 'NONE',  ( 0.000000000000000000, -0.9510565162951504226, -0.3090169943749573322 ) ) ;
#21693 = DIRECTION ( 'NONE',  ( 0.000000000000000000, -0.9510565162951503115, -0.3090169943749573322 ) ) ;
#21694 = ORIENTED_EDGE ( 'NONE', *, *, #14846, .T. ) ;
#21695 = CARTESIAN_POINT ( 'NONE',  ( 10.00000000000000000, 25.48117629651203941, -10.33947075754235989 ) ) ;
#21696 = ORIENTED_EDGE ( 'NONE', *, *, #4594, .F. ) ;
#21697 = EDGE_CURVE ( 'NONE', #11959, #21408, #2844, .T. ) ;
#21698 = ORIENTED_EDGE ( 'NONE', *, *, #7481, .T. ) ;
#21699 = CARTESIAN_POINT ( 'NONE',  ( 10.00000000000000000, -69.25892805976475586, -49.38005998797915908 ) ) ;
#21700 = ORIENTED_EDGE ( 'NONE', *, *, #3163, .T. ) ;
#21701 = ORIENTED_EDGE ( 'NONE', *, *, #19732, .T. ) ;
#21702 = CARTESIAN_POINT ( 'NONE',  ( -123.0000000000000000, 1.506315562951244531E-14, -3.000000000000000000 ) ) ;
#21703 = CARTESIAN_POINT ( 'NONE',  ( 0.000000000000000000, 25.17124263951009411, -12.69364185792227495 ) ) ;
#21704 = VERTEX_POINT ( 'NONE', #11241 ) ;
#21705 = AXIS2_PLACEMENT_3D ( 'NONE', #16989, #7375, #15760 ) ;
#21706 = AXIS2_PLACEMENT_3D ( 'NONE', #4456, #3014, #21150 ) ;
#21707 = DIRECTION ( 'NONE',  ( -1.000000000000000000, -0.000000000000000000, -0.000000000000000000 ) ) ;
#21708 = CARTESIAN_POINT ( 'NONE',  ( 10.00000000000000000, 0.000000000000000000, 0.000000000000000000 ) ) ;
#21709 = LINE ( 'NONE', #19831, #12905 ) ;
#21710 = CARTESIAN_POINT ( 'NONE',  ( 0.000000000000000000, 0.000000000000000000, 0.000000000000000000 ) ) ;
#21711 = CIRCLE ( 'NONE', #3006, 11.99999999999999822 ) ;
#21712 = CARTESIAN_POINT ( 'NONE',  ( 10.00000000000000000, 24.89070495400845573, -84.40647372620476574 ) ) ;
#21713 = DIRECTION ( 'NONE',  ( 0.000000000000000000, 0.000000000000000000, -1.000000000000000000 ) ) ;
#21714 = ORIENTED_EDGE ( 'NONE', *, *, #4869, .T. ) ;
#21715 = CYLINDRICAL_SURFACE ( 'NONE', #12694, 11.99999999999999822 ) ;
#21716 = DIRECTION ( 'NONE',  ( 0.000000000000000000, -0.9702957262759939194, -0.2419218955996776110 ) ) ;
#21717 = EDGE_CURVE ( 'NONE', #11505, #8089, #15800, .T. ) ;
#21718 = ORIENTED_EDGE ( 'NONE', *, *, #6691, .T. ) ;
#21719 = AXIS2_PLACEMENT_3D ( 'NONE', #6334, #899, #7644 ) ;
#21720 = AXIS2_PLACEMENT_3D ( 'NONE', #16395, #8122, #18177 ) ;
#21721 = CARTESIAN_POINT ( 'NONE',  ( 0.000000000000000000, 0.000000000000000000, 0.000000000000000000 ) ) ;
#21722 = VECTOR ( 'NONE', #17484, 1000.000000000000000 ) ;
#21723 = VERTEX_POINT ( 'NONE', #14662 ) ;
#21724 = FILL_AREA_STYLE_COLOUR ( '', #4937 ) ;
#21725 = DIRECTION ( 'NONE',  ( 0.000000000000000000, 0.000000000000000000, 1.000000000000000000 ) ) ;
#21726 = EDGE_LOOP ( 'NONE', ( #14199, #6394 ) ) ;
#21727 = EDGE_CURVE ( 'NONE', #10528, #7709, #1415, .T. ) ;
#21728 = DIRECTION ( 'NONE',  ( 1.000000000000000000, 0.000000000000000000, -0.000000000000000000 ) ) ;
#21729 = EDGE_LOOP ( 'NONE', ( #4394, #19854, #726, #1457 ) ) ;
#21730 = ORIENTED_EDGE ( 'NONE', *, *, #11716, .F. ) ;
#21731 = CARTESIAN_POINT ( 'NONE',  ( 5.000000000000002665, -79.38136668499764426, 37.98155635597287016 ) ) ;
#21732 = ORIENTED_EDGE ( 'NONE', *, *, #15940, .T. ) ;
#21733 = EDGE_CURVE ( 'NONE', #16240, #20720, #12718, .T. ) ;
#21734 = DIRECTION ( 'NONE',  ( 0.000000000000000000, 0.000000000000000000, 1.000000000000000000 ) ) ;
#21735 = LINE ( 'NONE', #4840, #11460 ) ;
#21736 = CARTESIAN_POINT ( 'NONE',  ( 5.000000000000002665, 6.797690662955227836, 87.73705831432218361 ) ) ;
#21737 = AXIS2_PLACEMENT_3D ( 'NONE', #16686, #11829, #13149 ) ;
#21738 = CARTESIAN_POINT ( 'NONE',  ( 0.000000000000000000, -15.25521607131190294, -23.70650506194185425 ) ) ;
#21739 = SURFACE_STYLE_FILL_AREA ( #19861 ) ;
#21740 = AXIS2_PLACEMENT_3D ( 'NONE', #5790, #14172, #12514 ) ;
#21741 = AXIS2_PLACEMENT_3D ( 'NONE', #6174, #1004, #14892 ) ;
#21742 = CARTESIAN_POINT ( 'NONE',  ( 0.000000000000000000, -68.36541360927154187, -50.60987712331774446 ) ) ;
#21743 = CARTESIAN_POINT ( 'NONE',  ( 0.000000000000000000, 5.000000000000004441, 0.000000000000000000 ) ) ;
#21744 = DIRECTION ( 'NONE',  ( -1.000000000000000000, -0.000000000000000000, -0.000000000000000000 ) ) ;
#21745 = EDGE_CURVE ( 'NONE', #17337, #2668, #6061, .T. ) ;
#21746 = DIRECTION ( 'NONE',  ( -1.000000000000000000, 0.000000000000000000, -0.000000000000000000 ) ) ;
#21747 = ADVANCED_FACE ( 'NONE', ( #17880 ), #16215, .F. ) ;
#21748 = EDGE_CURVE ( 'NONE', #8019, #14362, #3912, .T. ) ;
#21749 = DIRECTION ( 'NONE',  ( -1.000000000000000000, -0.000000000000000000, -0.000000000000000000 ) ) ;
#21750 = VERTEX_POINT ( 'NONE', #11133 ) ;
#21751 = ADVANCED_FACE ( 'NONE', ( #1076 ), #6170, .F. ) ;
#21752 = DIRECTION ( 'NONE',  ( 1.000000000000000000, 0.000000000000000000, 0.000000000000000000 ) ) ;
#21753 = CIRCLE ( 'NONE', #243, 32.00000000000000000 ) ;
#21754 = ORIENTED_EDGE ( 'NONE', *, *, #16212, .T. ) ;
#21755 = AXIS2_PLACEMENT_3D ( 'NONE', #13494, #10192, #5336 ) ;
#21756 = EDGE_LOOP ( 'NONE', ( #2163, #100, #19615, #19061 ) ) ;
#21757 = VERTEX_POINT ( 'NONE', #20512 ) ;
#21758 = VERTEX_POINT ( 'NONE', #20084 ) ;
#21759 = EDGE_CURVE ( 'NONE', #14362, #13200, #13657, .T. ) ;
#21760 = DIRECTION ( 'NONE',  ( 1.000000000000000000, 0.000000000000000000, 0.000000000000000000 ) ) ;
#21761 = VERTEX_POINT ( 'NONE', #4948 ) ;
#21762 = DIRECTION ( 'NONE',  ( 1.000000000000000000, 0.000000000000000000, 0.000000000000000000 ) ) ;
#21763 = EDGE_CURVE ( 'NONE', #13276, #7808, #10334, .T. ) ;
#21764 = AXIS2_PLACEMENT_3D ( 'NONE', #19454, #21010, #4312 ) ;
#21765 = CARTESIAN_POINT ( 'NONE',  ( 10.00000000000000000, 0.000000000000000000, 0.000000000000000000 ) ) ;
#21766 = VECTOR ( 'NONE', #13433, 1000.000000000000000 ) ;
#21767 = CARTESIAN_POINT ( 'NONE',  ( 0.000000000000000000, 33.95793648385932784, -86.04239391577952745 ) ) ;
#21768 = AXIS2_PLACEMENT_3D ( 'NONE', #1772, #11823, #15466 ) ;
#21769 = DIRECTION ( 'NONE',  ( 1.000000000000000000, 0.000000000000000000, 0.000000000000000000 ) ) ;
#21770 = CARTESIAN_POINT ( 'NONE',  ( 5.000000000000000000, 78.80192417387979731, -39.16958956249220591 ) ) ;
#21771 = ORIENTED_EDGE ( 'NONE', *, *, #2566, .F. ) ;
#21772 = DIRECTION ( 'NONE',  ( 0.000000000000000000, 0.000000000000000000, 1.000000000000000000 ) ) ;
#21773 = ADVANCED_FACE ( 'NONE', ( #8252 ), #8476, .F. ) ;
#21774 = ORIENTED_EDGE ( 'NONE', *, *, #12448, .T. ) ;
#21775 = ORIENTED_EDGE ( 'NONE', *, *, #3830, .F. ) ;
#21776 = VECTOR ( 'NONE', #11258, 1000.000000000000000 ) ;
#21777 = LINE ( 'NONE', #8092, #4598 ) ;
#21778 = ORIENTED_EDGE ( 'NONE', *, *, #7577, .T. ) ;
#21779 = AXIS2_PLACEMENT_3D ( 'NONE', #3921, #179, #3494 ) ;
#21780 = CARTESIAN_POINT ( 'NONE',  ( 10.00000000000000000, -78.04699792498111321, -49.64978465107371619 ) ) ;
#21781 = ORIENTED_EDGE ( 'NONE', *, *, #4884, .F. ) ;
#21782 = VERTEX_POINT ( 'NONE', #15419 ) ;
#21783 = AXIS2_PLACEMENT_3D ( 'NONE', #3187, #16661, #13561 ) ;
#21784 = ADVANCED_FACE ( 'NONE', ( #15202 ), #11783, .T. ) ;
#21785 = DIRECTION ( 'NONE',  ( -1.000000000000000000, -0.000000000000000000, -0.000000000000000000 ) ) ;
#21786 = VERTEX_POINT ( 'NONE', #16752 ) ;
#21787 = DIRECTION ( 'NONE',  ( 0.000000000000000000, 0.7431448254773908024, 0.6691306063588620123 ) ) ;
#21788 = EDGE_CURVE ( 'NONE', #6618, #8570, #10624, .T. ) ;
#21789 = DIRECTION ( 'NONE',  ( -1.000000000000000000, 0.000000000000000000, 0.000000000000000000 ) ) ;
#21790 = FACE_OUTER_BOUND ( 'NONE', #4389, .T. ) ;
#21791 = DIRECTION ( 'NONE',  ( 0.000000000000000000, 0.000000000000000000, 1.000000000000000000 ) ) ;
#21792 = DIRECTION ( 'NONE',  ( -1.000000000000000000, -0.000000000000000000, -0.000000000000000000 ) ) ;
#21793 = EDGE_CURVE ( 'NONE', #14824, #6420, #7450, .T. ) ;
#21794 = EDGE_CURVE ( 'NONE', #797, #21353, #13548, .T. ) ;
#21795 = CARTESIAN_POINT ( 'NONE',  ( 0.000000000000000000, -26.69209308833512395, 6.612652082459228531 ) ) ;
#21796 = DIRECTION ( 'NONE',  ( 0.000000000000000000, 0.000000000000000000, 1.000000000000000000 ) ) ;
#21797 = DIRECTION ( 'NONE',  ( 1.000000000000000000, 0.000000000000000000, 0.000000000000000000 ) ) ;
#21798 = SHAPE_REPRESENTATION ( 'center shaft', ( #15567 ), #3925 ) ;
#21799 = VECTOR ( 'NONE', #10230, 1000.000000000000000 ) ;
#21800 = AXIS2_PLACEMENT_3D ( 'NONE', #7473, #735, #6153 ) ;
#21801 = ORIENTED_EDGE ( 'NONE', *, *, #2179, .F. ) ;
#21802 = VECTOR ( 'NONE', #1802, 1000.000000000000000 ) ;
#21803 = CARTESIAN_POINT ( 'NONE',  ( 0.000000000000000000, -81.55207211302061410, -24.17537951050148592 ) ) ;
#21804 = DIRECTION ( 'NONE',  ( 0.000000000000000000, 0.000000000000000000, 1.000000000000000000 ) ) ;
#21805 = ORIENTED_EDGE ( 'NONE', *, *, #5270, .T. ) ;
#21806 = CARTESIAN_POINT ( 'NONE',  ( 0.000000000000000000, -85.05652083079338865, -0.7600687895868707411 ) ) ;
#21807 = ORIENTED_EDGE ( 'NONE', *, *, #21302, .T. ) ;
#21808 = CIRCLE ( 'NONE', #646, 92.50099999999999056 ) ;
#21809 = CIRCLE ( 'NONE', #16165, 9.999999999999998224 ) ;
#21810 = EDGE_LOOP ( 'NONE', ( #11101, #15268, #942, #2404 ) ) ;
#21811 = CARTESIAN_POINT ( 'NONE',  ( 0.000000000000000000, 4.294029059350239486, -27.86182539015961979 ) ) ;
#21812 = ORIENTED_EDGE ( 'NONE', *, *, #6135, .F. ) ;
#21813 = VECTOR ( 'NONE', #15718, 1000.000000000000000 ) ;
#21814 = VERTEX_POINT ( 'NONE', #20299 ) ;
#21815 = FACE_OUTER_BOUND ( 'NONE', #7805, .T. ) ;
#21816 = AXIS2_PLACEMENT_3D ( 'NONE', #19465, #20905, #12500 ) ;
#21817 = VERTEX_POINT ( 'NONE', #10120 ) ;
#21818 = AXIS2_PLACEMENT_3D ( 'NONE', #13146, #7967, #8081 ) ;
#21819 = EDGE_LOOP ( 'NONE', ( #2946, #19942, #15013, #8860 ) ) ;
#21820 = CARTESIAN_POINT ( 'NONE',  ( 5.000000000000000000, -0.6021240089803554518, 31.99433460282944708 ) ) ;
#21821 = DIRECTION ( 'NONE',  ( -1.000000000000000000, -0.000000000000000000, -0.000000000000000000 ) ) ;
#21822 = CARTESIAN_POINT ( 'NONE',  ( -1.400000000000000577, 9.062386313690438040E-16, 7.400000000000019895 ) ) ;
#21823 = FACE_OUTER_BOUND ( 'NONE', #3943, .T. ) ;
#21824 = CARTESIAN_POINT ( 'NONE',  ( 10.00000000000000000, 19.07277123396541185, 19.80970465344755027 ) ) ;
#21825 = CYLINDRICAL_SURFACE ( 'NONE', #11690, 6.728125000000023448 ) ;
#21826 = EDGE_LOOP ( 'NONE', ( #3933, #8357 ) ) ;
#21827 = DIRECTION ( 'NONE',  ( 0.000000000000000000, 0.000000000000000000, 1.000000000000000000 ) ) ;
#21828 = DIRECTION ( 'NONE',  ( 0.000000000000000000, 0.000000000000000000, 1.000000000000000000 ) ) ;
#21829 = ORIENTED_EDGE ( 'NONE', *, *, #8949, .T. ) ;
#21830 = STYLED_ITEM ( 'NONE', ( #16999 ), #20339 ) ;
#21831 = AXIS2_PLACEMENT_3D ( 'NONE', #1091, #21420, #9575 ) ;
#21832 = CARTESIAN_POINT ( 'NONE',  ( -10.00000000000000000, 0.000000000000000000, 0.000000000000000000 ) ) ;
#21833 = ORIENTED_EDGE ( 'NONE', *, *, #12983, .F. ) ;
#21834 = CARTESIAN_POINT ( 'NONE',  ( -90.00000000000000000, 1.393954219129475159E-14, 113.8250000000000171 ) ) ;
#21835 = DIRECTION ( 'NONE',  ( 0.000000000000000000, 0.000000000000000000, 1.000000000000000000 ) ) ;
#21836 = VERTEX_POINT ( 'NONE', #16979 ) ;
#21837 = CARTESIAN_POINT ( 'NONE',  ( 0.000000000000000000, 0.000000000000000000, 0.000000000000000000 ) ) ;
#21838 = ORIENTED_EDGE ( 'NONE', *, *, #15131, .T. ) ;
#21839 = ORIENTED_EDGE ( 'NONE', *, *, #21116, .F. ) ;
#21840 = VERTEX_POINT ( 'NONE', #1623 ) ;
#21841 = FACE_OUTER_BOUND ( 'NONE', #14687, .T. ) ;
#21842 = ORIENTED_EDGE ( 'NONE', *, *, #11627, .T. ) ;
#21843 = DIRECTION ( 'NONE',  ( -1.000000000000000000, -0.000000000000000000, 0.000000000000000000 ) ) ;
#21844 = CIRCLE ( 'NONE', #19027, 44.99999999999999289 ) ;
#21845 = DIRECTION ( 'NONE',  ( -1.000000000000000000, 0.000000000000000000, -0.000000000000000000 ) ) ;
#21846 = DIRECTION ( 'NONE',  ( 0.000000000000000000, 0.000000000000000000, 1.000000000000000000 ) ) ;
#21847 = EDGE_CURVE ( 'NONE', #15418, #13049, #10974, .T. ) ;
#21848 = AXIS2_PLACEMENT_3D ( 'NONE', #14880, #1506, #18529 ) ;
#21849 = DIRECTION ( 'NONE',  ( -1.000000000000000000, 0.000000000000000000, 0.000000000000000000 ) ) ;
#21850 = AXIS2_PLACEMENT_3D ( 'NONE', #394, #7246, #17406 ) ;
#21852 = AXIS2_PLACEMENT_3D ( 'NONE', #12553, #8905, #740 ) ;
#21851 = PRODUCT_DEFINITION_SHAPE ( 'NONE', 'NONE',  #12508 ) ;
#21853 = DIRECTION ( 'NONE',  ( 0.000000000000000000, -0.6946583704590034714, 0.7193398003386451967 ) ) ;
#21854 = DIRECTION ( 'NONE',  ( 0.000000000000000000, 0.000000000000000000, 1.000000000000000000 ) ) ;
#21855 = LINE ( 'NONE', #6954, #9967 ) ;
#21856 = ADVANCED_FACE ( 'NONE', ( #1733 ), #5165, .F. ) ;
#21857 = EDGE_LOOP ( 'NONE', ( #18854, #10448, #16431, #3354 ) ) ;
#21858 = NEXT_ASSEMBLY_USAGE_OCCURRENCE ( 'NAUO1', ' ', ' ', #12508, #101, $ ) ;
#21859 = NEXT_ASSEMBLY_USAGE_OCCURRENCE ( 'NAUO2', ' ', ' ', #12508, #5646, $ ) ;
#21860 = NEXT_ASSEMBLY_USAGE_OCCURRENCE ( 'NAUO3', ' ', ' ', #12508, #5916, $ ) ;
#21861 = NEXT_ASSEMBLY_USAGE_OCCURRENCE ( 'NAUO4', ' ', ' ', #12508, #3340, $ ) ;
#21862 = NEXT_ASSEMBLY_USAGE_OCCURRENCE ( 'NAUO5', ' ', ' ', #12508, #4011, $ ) ;
#21863 = NEXT_ASSEMBLY_USAGE_OCCURRENCE ( 'NAUO6', ' ', ' ', #12508, #19678, $ ) ;
#21864 = NEXT_ASSEMBLY_USAGE_OCCURRENCE ( 'NAUO7', ' ', ' ', #12508, #9257, $ ) ;
#21865 = NEXT_ASSEMBLY_USAGE_OCCURRENCE ( 'NAUO8', ' ', ' ', #12508, #381, $ ) ;
#21866 = NEXT_ASSEMBLY_USAGE_OCCURRENCE ( 'NAUO9', ' ', ' ', #12508, #9257, $ ) ;
ENDSEC;
END-ISO-10303-21;
